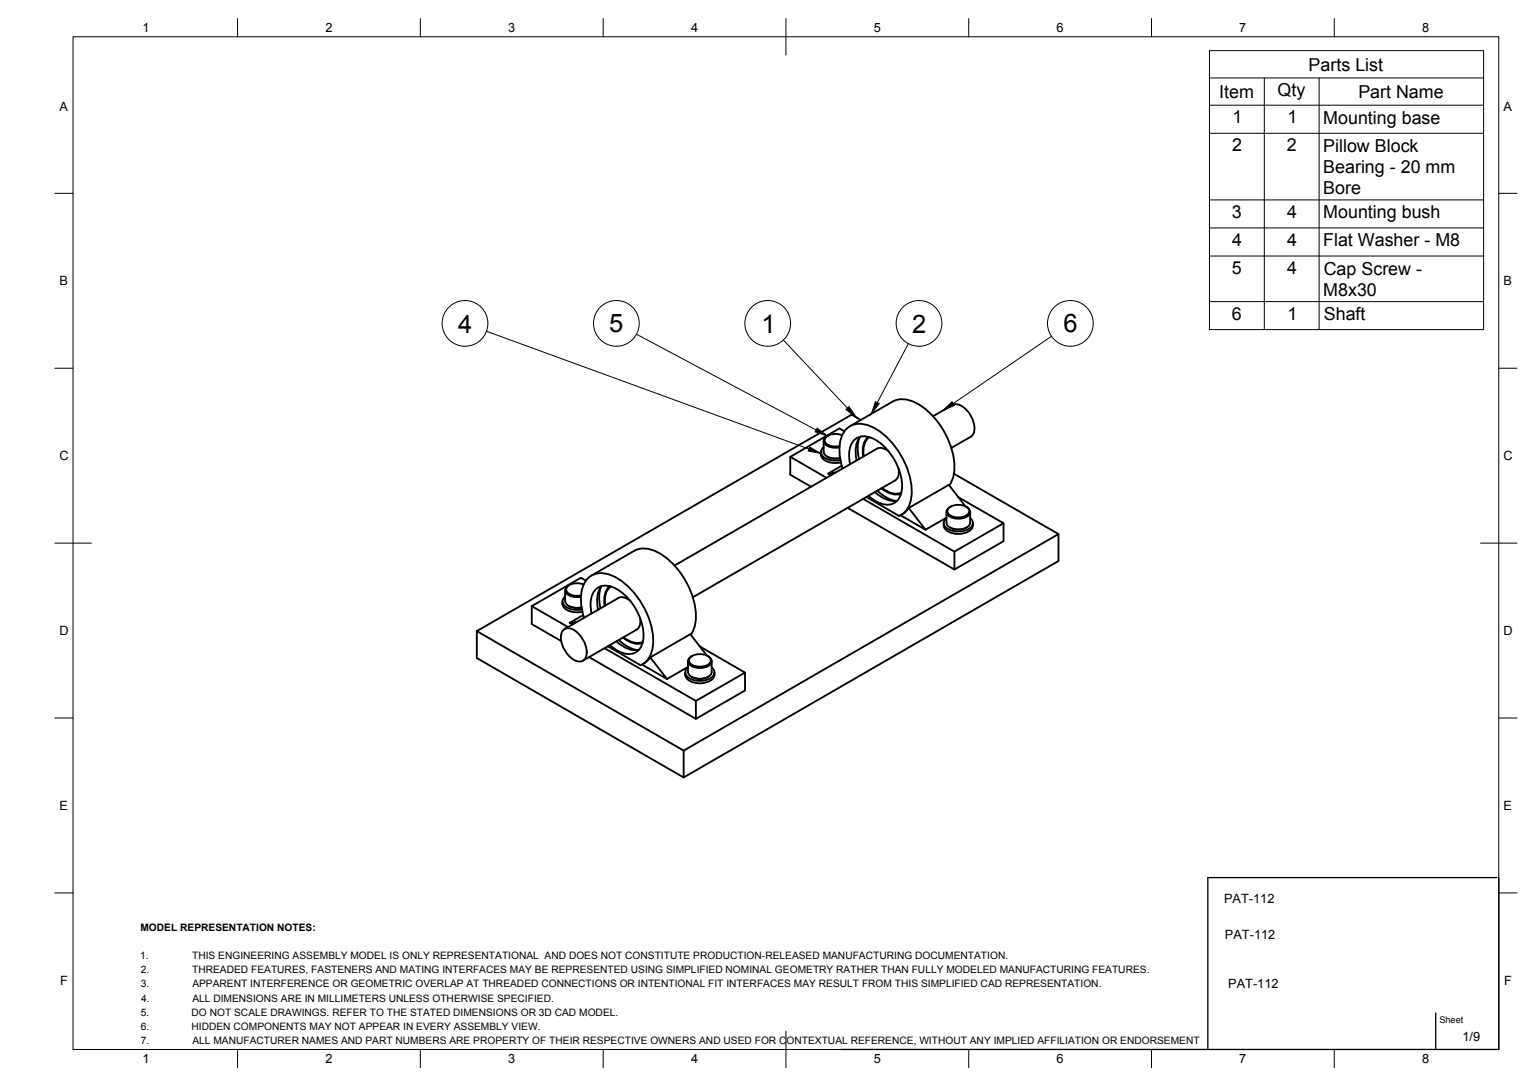
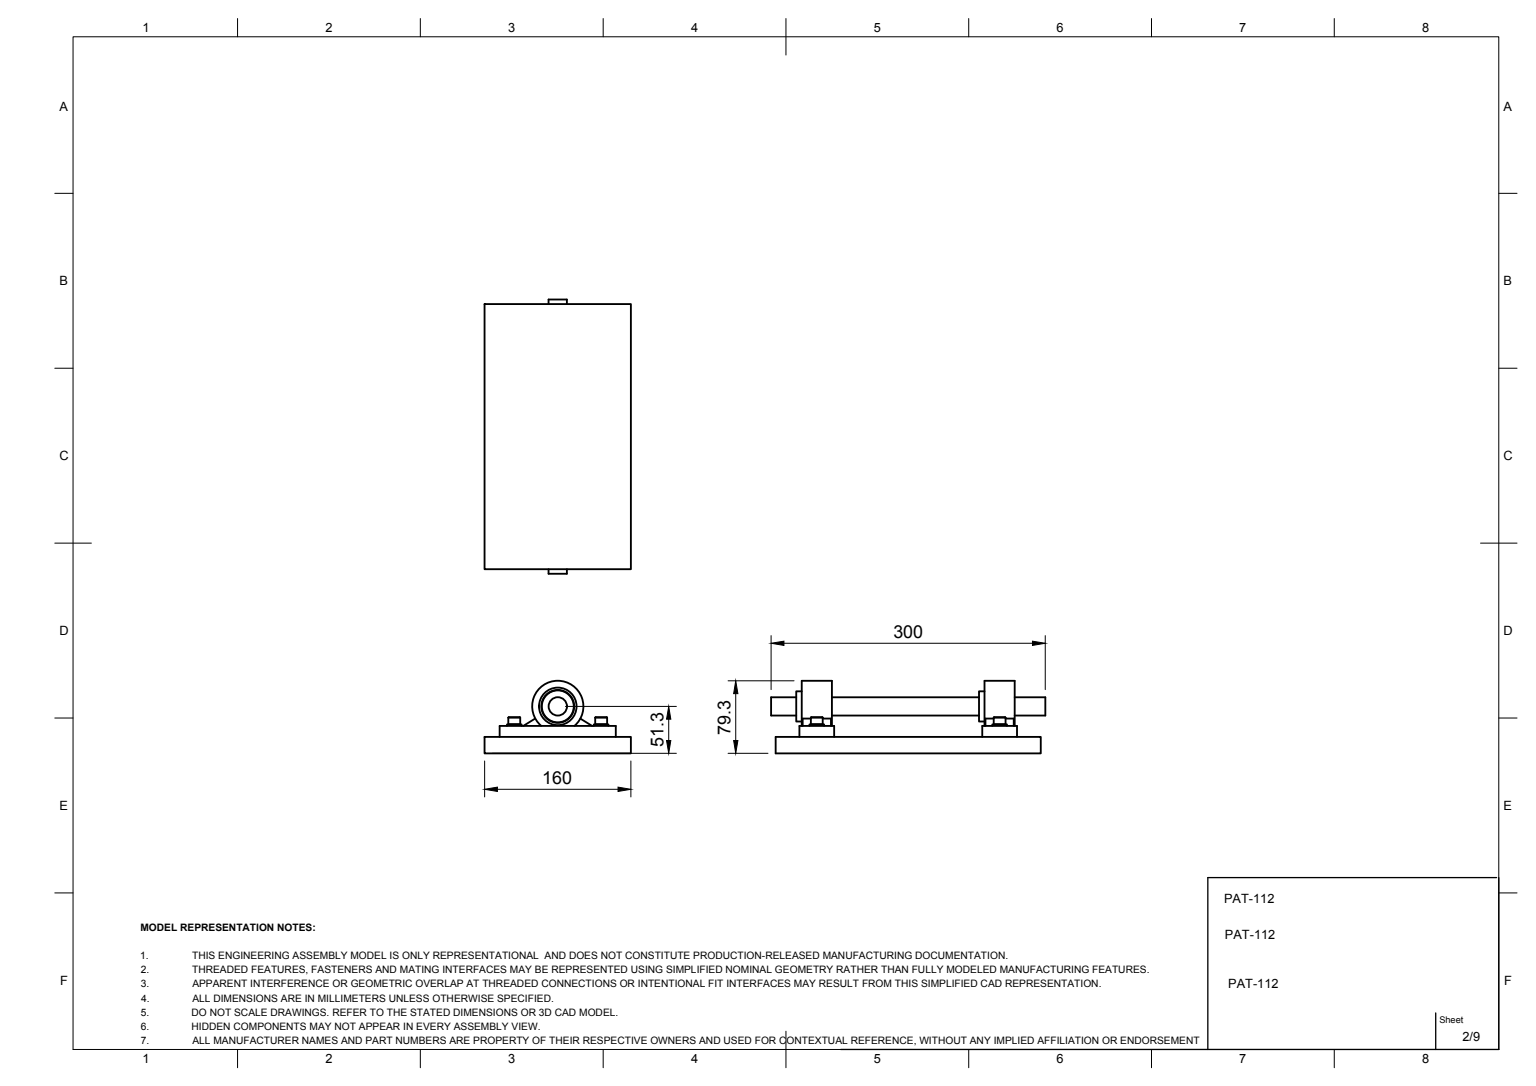
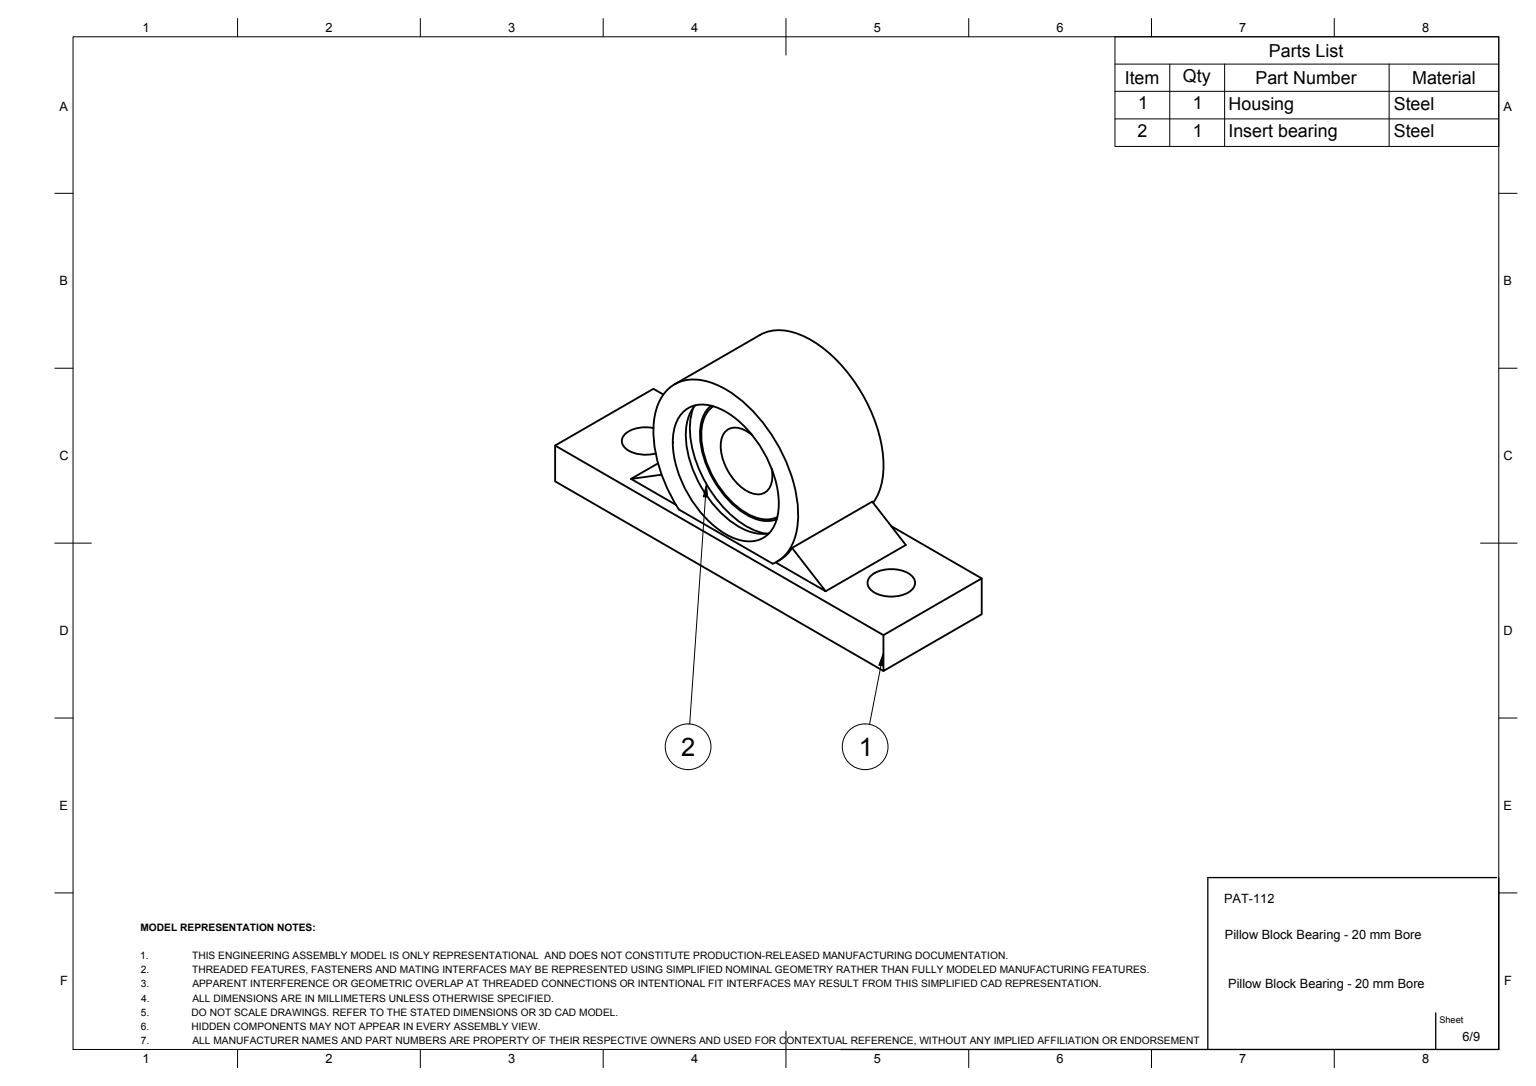
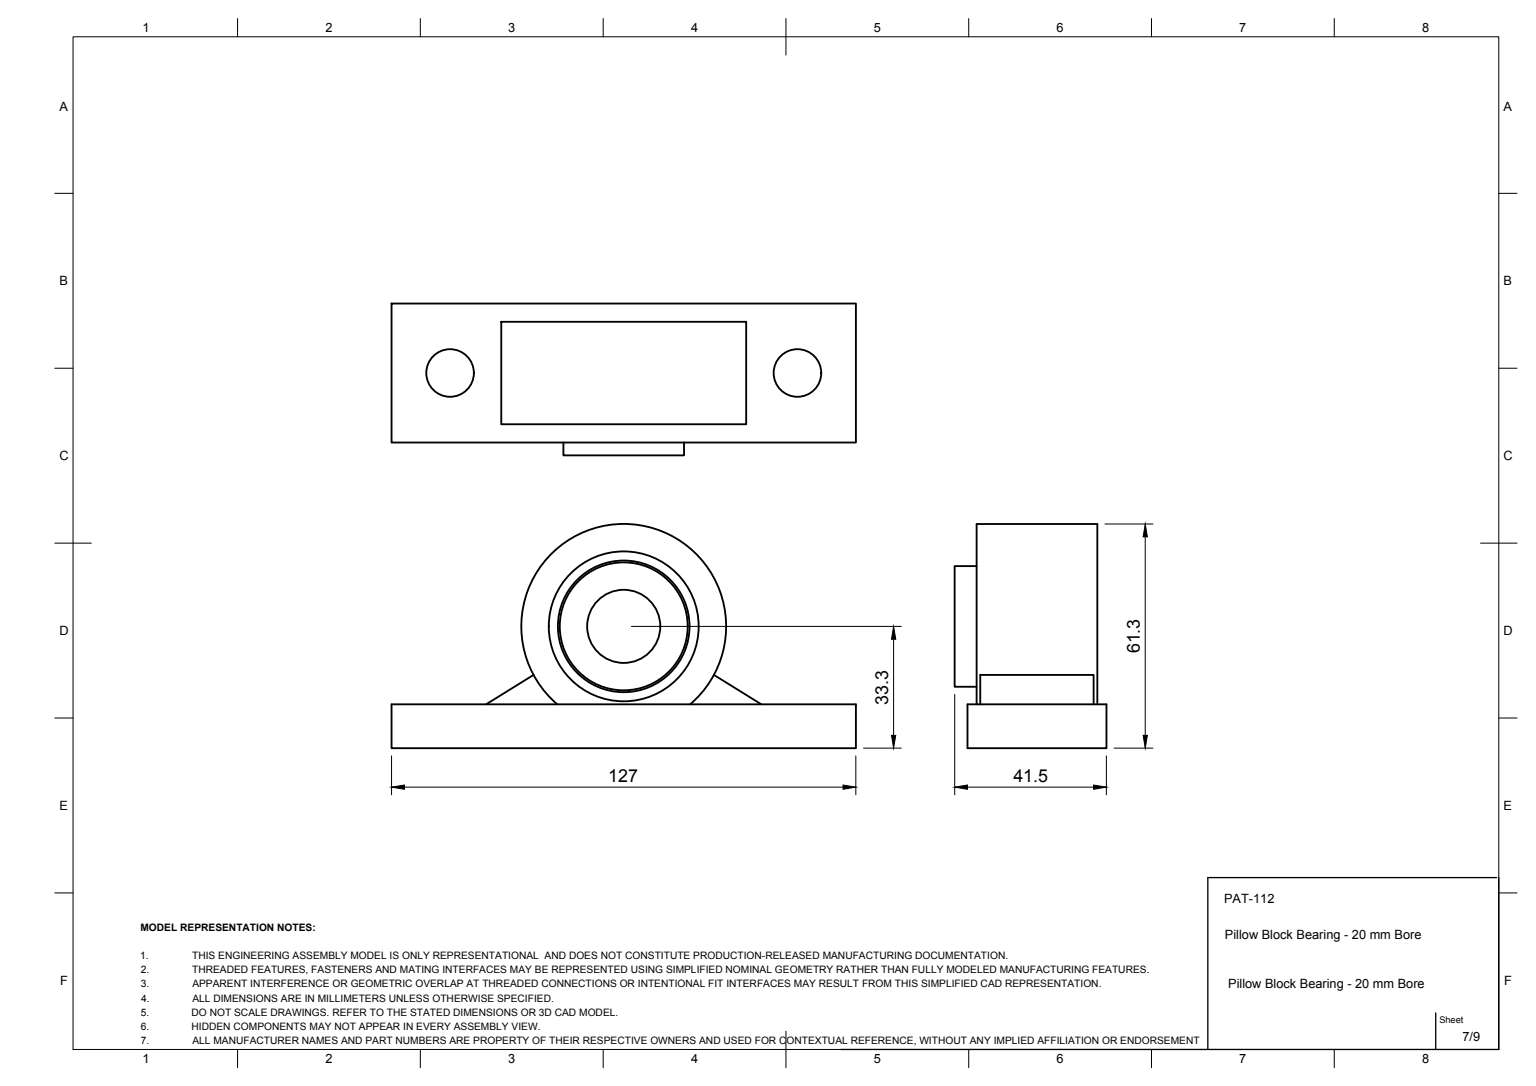
ISO-10303-21;
HEADER;
/* Generated by software containing ST-Developer
 * from STEP Tools, Inc. (www.steptools.com) 
 */

FILE_DESCRIPTION(
/* description */ ('PAT-112'),
/* implementation_level */ '2;1');

FILE_NAME(
/* name */ 'PAT-112.step',
/* time_stamp */ '2026-11-15T15:25:42-08:00',
/* author */ (''),
/* organization */ (''),
/* preprocessor_version */ 'ST-DEVELOPER v20.2',
/* originating_system */ 'Autodesk Translation Framework v15.17.0.0',
/* authorisation */ '');

FILE_SCHEMA (('AUTOMOTIVE_DESIGN { 1 0 10303 214 3 1 1 }'));
ENDSEC;

DATA;
#10=MECHANICAL_DESIGN_GEOMETRIC_PRESENTATION_REPRESENTATION('',(#105,#106,
#107,#108,#109,#110,#111,#112),#2277);
#11=CONICAL_SURFACE('',#1463,0.625,0.785398163397448);
#12=CONICAL_SURFACE('',#1467,0.635,0.785398163397449);
#13=CONICAL_SURFACE('',#1471,0.41,0.463647609000806);
#14=CONICAL_SURFACE('',#1475,0.36,0.785398163397448);
#15=ORIENTED_CLOSED_SHELL('',*,#1263,.F.);
#16=BREP_WITH_VOIDS('Body1',#1264,(#15));
#17=ITEM_DEFINED_TRANSFORMATION($,$,#1369,#1432);
#18=ITEM_DEFINED_TRANSFORMATION($,$,#1410,#1433);
#19=ITEM_DEFINED_TRANSFORMATION($,$,#1345,#1484);
#20=ITEM_DEFINED_TRANSFORMATION($,$,#1368,#1485);
#21=ITEM_DEFINED_TRANSFORMATION($,$,#1434,#1486);
#22=ITEM_DEFINED_TRANSFORMATION($,$,#1443,#1487);
#23=ITEM_DEFINED_TRANSFORMATION($,$,#1452,#1488);
#24=ITEM_DEFINED_TRANSFORMATION($,$,#1434,#1489);
#25=ITEM_DEFINED_TRANSFORMATION($,$,#1443,#1490);
#26=ITEM_DEFINED_TRANSFORMATION($,$,#1452,#1491);
#27=ITEM_DEFINED_TRANSFORMATION($,$,#1368,#1492);
#28=ITEM_DEFINED_TRANSFORMATION($,$,#1434,#1493);
#29=ITEM_DEFINED_TRANSFORMATION($,$,#1443,#1494);
#30=ITEM_DEFINED_TRANSFORMATION($,$,#1452,#1495);
#31=ITEM_DEFINED_TRANSFORMATION($,$,#1434,#1496);
#32=ITEM_DEFINED_TRANSFORMATION($,$,#1443,#1497);
#33=ITEM_DEFINED_TRANSFORMATION($,$,#1452,#1498);
#34=ITEM_DEFINED_TRANSFORMATION($,$,#1478,#1499);
#35=(
REPRESENTATION_RELATIONSHIP($,$,#2321,#2320)
REPRESENTATION_RELATIONSHIP_WITH_TRANSFORMATION(#17)
SHAPE_REPRESENTATION_RELATIONSHIP()
);
#36=(
REPRESENTATION_RELATIONSHIP($,$,#2322,#2320)
REPRESENTATION_RELATIONSHIP_WITH_TRANSFORMATION(#18)
SHAPE_REPRESENTATION_RELATIONSHIP()
);
#37=(
REPRESENTATION_RELATIONSHIP($,$,#2319,#2318)
REPRESENTATION_RELATIONSHIP_WITH_TRANSFORMATION(#19)
SHAPE_REPRESENTATION_RELATIONSHIP()
);
#38=(
REPRESENTATION_RELATIONSHIP($,$,#2320,#2318)
REPRESENTATION_RELATIONSHIP_WITH_TRANSFORMATION(#20)
SHAPE_REPRESENTATION_RELATIONSHIP()
);
#39=(
REPRESENTATION_RELATIONSHIP($,$,#2323,#2318)
REPRESENTATION_RELATIONSHIP_WITH_TRANSFORMATION(#21)
SHAPE_REPRESENTATION_RELATIONSHIP()
);
#40=(
REPRESENTATION_RELATIONSHIP($,$,#2324,#2318)
REPRESENTATION_RELATIONSHIP_WITH_TRANSFORMATION(#22)
SHAPE_REPRESENTATION_RELATIONSHIP()
);
#41=(
REPRESENTATION_RELATIONSHIP($,$,#2325,#2318)
REPRESENTATION_RELATIONSHIP_WITH_TRANSFORMATION(#23)
SHAPE_REPRESENTATION_RELATIONSHIP()
);
#42=(
REPRESENTATION_RELATIONSHIP($,$,#2323,#2318)
REPRESENTATION_RELATIONSHIP_WITH_TRANSFORMATION(#24)
SHAPE_REPRESENTATION_RELATIONSHIP()
);
#43=(
REPRESENTATION_RELATIONSHIP($,$,#2324,#2318)
REPRESENTATION_RELATIONSHIP_WITH_TRANSFORMATION(#25)
SHAPE_REPRESENTATION_RELATIONSHIP()
);
#44=(
REPRESENTATION_RELATIONSHIP($,$,#2325,#2318)
REPRESENTATION_RELATIONSHIP_WITH_TRANSFORMATION(#26)
SHAPE_REPRESENTATION_RELATIONSHIP()
);
#45=(
REPRESENTATION_RELATIONSHIP($,$,#2320,#2318)
REPRESENTATION_RELATIONSHIP_WITH_TRANSFORMATION(#27)
SHAPE_REPRESENTATION_RELATIONSHIP()
);
#46=(
REPRESENTATION_RELATIONSHIP($,$,#2323,#2318)
REPRESENTATION_RELATIONSHIP_WITH_TRANSFORMATION(#28)
SHAPE_REPRESENTATION_RELATIONSHIP()
);
#47=(
REPRESENTATION_RELATIONSHIP($,$,#2324,#2318)
REPRESENTATION_RELATIONSHIP_WITH_TRANSFORMATION(#29)
SHAPE_REPRESENTATION_RELATIONSHIP()
);
#48=(
REPRESENTATION_RELATIONSHIP($,$,#2325,#2318)
REPRESENTATION_RELATIONSHIP_WITH_TRANSFORMATION(#30)
SHAPE_REPRESENTATION_RELATIONSHIP()
);
#49=(
REPRESENTATION_RELATIONSHIP($,$,#2323,#2318)
REPRESENTATION_RELATIONSHIP_WITH_TRANSFORMATION(#31)
SHAPE_REPRESENTATION_RELATIONSHIP()
);
#50=(
REPRESENTATION_RELATIONSHIP($,$,#2324,#2318)
REPRESENTATION_RELATIONSHIP_WITH_TRANSFORMATION(#32)
SHAPE_REPRESENTATION_RELATIONSHIP()
);
#51=(
REPRESENTATION_RELATIONSHIP($,$,#2325,#2318)
REPRESENTATION_RELATIONSHIP_WITH_TRANSFORMATION(#33)
SHAPE_REPRESENTATION_RELATIONSHIP()
);
#52=(
REPRESENTATION_RELATIONSHIP($,$,#2326,#2318)
REPRESENTATION_RELATIONSHIP_WITH_TRANSFORMATION(#34)
SHAPE_REPRESENTATION_RELATIONSHIP()
);
#53=CONTEXT_DEPENDENT_SHAPE_REPRESENTATION(#35,#2296);
#54=CONTEXT_DEPENDENT_SHAPE_REPRESENTATION(#36,#2297);
#55=CONTEXT_DEPENDENT_SHAPE_REPRESENTATION(#37,#2302);
#56=CONTEXT_DEPENDENT_SHAPE_REPRESENTATION(#38,#2303);
#57=CONTEXT_DEPENDENT_SHAPE_REPRESENTATION(#39,#2304);
#58=CONTEXT_DEPENDENT_SHAPE_REPRESENTATION(#40,#2305);
#59=CONTEXT_DEPENDENT_SHAPE_REPRESENTATION(#41,#2306);
#60=CONTEXT_DEPENDENT_SHAPE_REPRESENTATION(#42,#2307);
#61=CONTEXT_DEPENDENT_SHAPE_REPRESENTATION(#43,#2308);
#62=CONTEXT_DEPENDENT_SHAPE_REPRESENTATION(#44,#2309);
#63=CONTEXT_DEPENDENT_SHAPE_REPRESENTATION(#45,#2310);
#64=CONTEXT_DEPENDENT_SHAPE_REPRESENTATION(#46,#2311);
#65=CONTEXT_DEPENDENT_SHAPE_REPRESENTATION(#47,#2312);
#66=CONTEXT_DEPENDENT_SHAPE_REPRESENTATION(#48,#2313);
#67=CONTEXT_DEPENDENT_SHAPE_REPRESENTATION(#49,#2314);
#68=CONTEXT_DEPENDENT_SHAPE_REPRESENTATION(#50,#2315);
#69=CONTEXT_DEPENDENT_SHAPE_REPRESENTATION(#51,#2316);
#70=CONTEXT_DEPENDENT_SHAPE_REPRESENTATION(#52,#2317);
#71=NEXT_ASSEMBLY_USAGE_OCCURRENCE('Housing:1','Housing:1','Housing:1',
#2330,#2331,'Housing:1');
#72=NEXT_ASSEMBLY_USAGE_OCCURRENCE('Insert bearing:1',
'Insert bearing:1','Insert bearing:1',#2330,#2332,'Insert bearing:1');
#73=NEXT_ASSEMBLY_USAGE_OCCURRENCE('Mounting base:1','Mounting base:1',
'Mounting base:1',#2328,#2329,'Mounting base:1');
#74=NEXT_ASSEMBLY_USAGE_OCCURRENCE(
'Pillow Block Bearing - 20 mm Bore:1',
'Pillow Block Bearing - 20 mm Bore:1',
'Pillow Block Bearing - 20 mm Bore:1',#2328,#2330,
'Pillow Block Bearing - 20 mm Bore:1');
#75=NEXT_ASSEMBLY_USAGE_OCCURRENCE('Mounting bush:1','Mounting bush:1',
'Mounting bush:1',#2328,#2333,'Mounting bush:1');
#76=NEXT_ASSEMBLY_USAGE_OCCURRENCE('Flat Washer - M8:1',
'Flat Washer - M8:1','Flat Washer - M8:1',#2328,#2334,
'Flat Washer - M8:1');
#77=NEXT_ASSEMBLY_USAGE_OCCURRENCE('Cap Screw - M8x30:1',
'Cap Screw - M8x30:1','Cap Screw - M8x30:1',#2328,#2335,
'Cap Screw - M8x30:1');
#78=NEXT_ASSEMBLY_USAGE_OCCURRENCE('Mounting bush:2','Mounting bush:2',
'Mounting bush:2',#2328,#2333,'Mounting bush:2');
#79=NEXT_ASSEMBLY_USAGE_OCCURRENCE('Flat Washer - M8:2',
'Flat Washer - M8:2','Flat Washer - M8:2',#2328,#2334,
'Flat Washer - M8:2');
#80=NEXT_ASSEMBLY_USAGE_OCCURRENCE('Cap Screw - M8x30:2',
'Cap Screw - M8x30:2','Cap Screw - M8x30:2',#2328,#2335,
'Cap Screw - M8x30:2');
#81=NEXT_ASSEMBLY_USAGE_OCCURRENCE(
'Pillow Block Bearing - 20 mm Bore:2',
'Pillow Block Bearing - 20 mm Bore:2',
'Pillow Block Bearing - 20 mm Bore:2',#2328,#2330,
'Pillow Block Bearing - 20 mm Bore:2');
#82=NEXT_ASSEMBLY_USAGE_OCCURRENCE('Mounting bush:3','Mounting bush:3',
'Mounting bush:3',#2328,#2333,'Mounting bush:3');
#83=NEXT_ASSEMBLY_USAGE_OCCURRENCE('Flat Washer - M8:3',
'Flat Washer - M8:3','Flat Washer - M8:3',#2328,#2334,
'Flat Washer - M8:3');
#84=NEXT_ASSEMBLY_USAGE_OCCURRENCE('Cap Screw - M8x30:3',
'Cap Screw - M8x30:3','Cap Screw - M8x30:3',#2328,#2335,
'Cap Screw - M8x30:3');
#85=NEXT_ASSEMBLY_USAGE_OCCURRENCE('Mounting bush:4','Mounting bush:4',
'Mounting bush:4',#2328,#2333,'Mounting bush:4');
#86=NEXT_ASSEMBLY_USAGE_OCCURRENCE('Flat Washer - M8:4',
'Flat Washer - M8:4','Flat Washer - M8:4',#2328,#2334,
'Flat Washer - M8:4');
#87=NEXT_ASSEMBLY_USAGE_OCCURRENCE('Cap Screw - M8x30:4',
'Cap Screw - M8x30:4','Cap Screw - M8x30:4',#2328,#2335,
'Cap Screw - M8x30:4');
#88=NEXT_ASSEMBLY_USAGE_OCCURRENCE('Shaft:1','Shaft:1','Shaft:1',#2328,
#2336,'Shaft:1');
#89=SPHERICAL_SURFACE('',#1376,2.35);
#90=SPHERICAL_SURFACE('',#1416,2.35);
#91=SHAPE_REPRESENTATION_RELATIONSHIP('SRR','None',#2319,#98);
#92=SHAPE_REPRESENTATION_RELATIONSHIP('SRR','None',#2321,#99);
#93=SHAPE_REPRESENTATION_RELATIONSHIP('SRR','None',#2322,#100);
#94=SHAPE_REPRESENTATION_RELATIONSHIP('SRR','None',#2323,#101);
#95=SHAPE_REPRESENTATION_RELATIONSHIP('SRR','None',#2324,#102);
#96=SHAPE_REPRESENTATION_RELATIONSHIP('SRR','None',#2325,#103);
#97=SHAPE_REPRESENTATION_RELATIONSHIP('SRR','None',#2326,#104);
#98=ADVANCED_BREP_SHAPE_REPRESENTATION('',(#113),#2269);
#99=ADVANCED_BREP_SHAPE_REPRESENTATION('',(#114),#2271);
#100=ADVANCED_BREP_SHAPE_REPRESENTATION('',(#115,#116),#2272);
#101=ADVANCED_BREP_SHAPE_REPRESENTATION('',(#117),#2273);
#102=ADVANCED_BREP_SHAPE_REPRESENTATION('',(#118),#2274);
#103=ADVANCED_BREP_SHAPE_REPRESENTATION('',(#16),#2275);
#104=ADVANCED_BREP_SHAPE_REPRESENTATION('',(#119),#2276);
#105=STYLED_ITEM('',(#2368),#113);
#106=STYLED_ITEM('',(#2368),#114);
#107=STYLED_ITEM('',(#2369),#115);
#108=STYLED_ITEM('',(#2369),#116);
#109=STYLED_ITEM('',(#2370),#117);
#110=STYLED_ITEM('',(#2371),#118);
#111=STYLED_ITEM('',(#2371),#16);
#112=STYLED_ITEM('',(#2367),#119);
#113=MANIFOLD_SOLID_BREP('Body1',#1257);
#114=MANIFOLD_SOLID_BREP('Body1',#1258);
#115=MANIFOLD_SOLID_BREP('Body1',#1259);
#116=MANIFOLD_SOLID_BREP('Body2',#1260);
#117=MANIFOLD_SOLID_BREP('Body1',#1261);
#118=MANIFOLD_SOLID_BREP('Body1',#1262);
#119=MANIFOLD_SOLID_BREP('Body1',#1265);
#120=FACE_BOUND('',#287,.T.);
#121=FACE_BOUND('',#288,.T.);
#122=FACE_BOUND('',#289,.T.);
#123=FACE_BOUND('',#290,.T.);
#124=FACE_BOUND('',#295,.T.);
#125=FACE_BOUND('',#296,.T.);
#126=FACE_BOUND('',#304,.T.);
#127=FACE_BOUND('',#305,.T.);
#128=FACE_BOUND('',#306,.T.);
#129=FACE_BOUND('',#309,.T.);
#130=FACE_BOUND('',#311,.T.);
#131=FACE_BOUND('',#324,.T.);
#132=FACE_BOUND('',#325,.T.);
#133=FACE_BOUND('',#326,.T.);
#134=FACE_BOUND('',#329,.T.);
#135=FACE_BOUND('',#331,.T.);
#136=FACE_BOUND('',#332,.T.);
#137=FACE_BOUND('',#334,.T.);
#138=FACE_BOUND('',#337,.T.);
#139=FACE_BOUND('',#339,.T.);
#140=FACE_BOUND('',#342,.T.);
#141=FACE_BOUND('',#347,.T.);
#142=FACE_BOUND('',#349,.T.);
#143=FACE_BOUND('',#353,.T.);
#144=FACE_BOUND('',#355,.T.);
#145=FACE_BOUND('',#369,.T.);
#146=PLANE('',#1349);
#147=PLANE('',#1353);
#148=PLANE('',#1357);
#149=PLANE('',#1361);
#150=PLANE('',#1362);
#151=PLANE('',#1363);
#152=PLANE('',#1364);
#153=PLANE('',#1365);
#154=PLANE('',#1366);
#155=PLANE('',#1367);
#156=PLANE('',#1378);
#157=PLANE('',#1380);
#158=PLANE('',#1382);
#159=PLANE('',#1384);
#160=PLANE('',#1385);
#161=PLANE('',#1387);
#162=PLANE('',#1388);
#163=PLANE('',#1394);
#164=PLANE('',#1395);
#165=PLANE('',#1396);
#166=PLANE('',#1397);
#167=PLANE('',#1398);
#168=PLANE('',#1399);
#169=PLANE('',#1400);
#170=PLANE('',#1405);
#171=PLANE('',#1406);
#172=PLANE('',#1407);
#173=PLANE('',#1408);
#174=PLANE('',#1409);
#175=PLANE('',#1414);
#176=PLANE('',#1419);
#177=PLANE('',#1423);
#178=PLANE('',#1425);
#179=PLANE('',#1429);
#180=PLANE('',#1441);
#181=PLANE('',#1442);
#182=PLANE('',#1450);
#183=PLANE('',#1451);
#184=PLANE('',#1453);
#185=PLANE('',#1454);
#186=PLANE('',#1455);
#187=PLANE('',#1456);
#188=PLANE('',#1457);
#189=PLANE('',#1458);
#190=PLANE('',#1459);
#191=PLANE('',#1460);
#192=PLANE('',#1461);
#193=PLANE('',#1469);
#194=PLANE('',#1477);
#195=PLANE('',#1479);
#196=PLANE('',#1483);
#197=FACE_OUTER_BOUND('',#274,.T.);
#198=FACE_OUTER_BOUND('',#275,.T.);
#199=FACE_OUTER_BOUND('',#276,.T.);
#200=FACE_OUTER_BOUND('',#277,.T.);
#201=FACE_OUTER_BOUND('',#278,.T.);
#202=FACE_OUTER_BOUND('',#279,.T.);
#203=FACE_OUTER_BOUND('',#280,.T.);
#204=FACE_OUTER_BOUND('',#281,.T.);
#205=FACE_OUTER_BOUND('',#282,.T.);
#206=FACE_OUTER_BOUND('',#283,.T.);
#207=FACE_OUTER_BOUND('',#284,.T.);
#208=FACE_OUTER_BOUND('',#285,.T.);
#209=FACE_OUTER_BOUND('',#286,.T.);
#210=FACE_OUTER_BOUND('',#291,.T.);
#211=FACE_OUTER_BOUND('',#292,.T.);
#212=FACE_OUTER_BOUND('',#293,.T.);
#213=FACE_OUTER_BOUND('',#294,.T.);
#214=FACE_OUTER_BOUND('',#297,.T.);
#215=FACE_OUTER_BOUND('',#298,.T.);
#216=FACE_OUTER_BOUND('',#299,.T.);
#217=FACE_OUTER_BOUND('',#300,.T.);
#218=FACE_OUTER_BOUND('',#301,.T.);
#219=FACE_OUTER_BOUND('',#302,.T.);
#220=FACE_OUTER_BOUND('',#303,.T.);
#221=FACE_OUTER_BOUND('',#307,.T.);
#222=FACE_OUTER_BOUND('',#308,.T.);
#223=FACE_OUTER_BOUND('',#310,.T.);
#224=FACE_OUTER_BOUND('',#312,.T.);
#225=FACE_OUTER_BOUND('',#313,.T.);
#226=FACE_OUTER_BOUND('',#314,.T.);
#227=FACE_OUTER_BOUND('',#315,.T.);
#228=FACE_OUTER_BOUND('',#316,.T.);
#229=FACE_OUTER_BOUND('',#317,.T.);
#230=FACE_OUTER_BOUND('',#318,.T.);
#231=FACE_OUTER_BOUND('',#319,.T.);
#232=FACE_OUTER_BOUND('',#320,.T.);
#233=FACE_OUTER_BOUND('',#321,.T.);
#234=FACE_OUTER_BOUND('',#322,.T.);
#235=FACE_OUTER_BOUND('',#323,.T.);
#236=FACE_OUTER_BOUND('',#327,.T.);
#237=FACE_OUTER_BOUND('',#328,.T.);
#238=FACE_OUTER_BOUND('',#330,.T.);
#239=FACE_OUTER_BOUND('',#333,.T.);
#240=FACE_OUTER_BOUND('',#335,.T.);
#241=FACE_OUTER_BOUND('',#336,.T.);
#242=FACE_OUTER_BOUND('',#338,.T.);
#243=FACE_OUTER_BOUND('',#340,.T.);
#244=FACE_OUTER_BOUND('',#341,.T.);
#245=FACE_OUTER_BOUND('',#343,.T.);
#246=FACE_OUTER_BOUND('',#344,.T.);
#247=FACE_OUTER_BOUND('',#345,.T.);
#248=FACE_OUTER_BOUND('',#346,.T.);
#249=FACE_OUTER_BOUND('',#348,.T.);
#250=FACE_OUTER_BOUND('',#350,.T.);
#251=FACE_OUTER_BOUND('',#351,.T.);
#252=FACE_OUTER_BOUND('',#352,.T.);
#253=FACE_OUTER_BOUND('',#354,.T.);
#254=FACE_OUTER_BOUND('',#356,.T.);
#255=FACE_OUTER_BOUND('',#357,.T.);
#256=FACE_OUTER_BOUND('',#358,.T.);
#257=FACE_OUTER_BOUND('',#359,.T.);
#258=FACE_OUTER_BOUND('',#360,.T.);
#259=FACE_OUTER_BOUND('',#361,.T.);
#260=FACE_OUTER_BOUND('',#362,.T.);
#261=FACE_OUTER_BOUND('',#363,.T.);
#262=FACE_OUTER_BOUND('',#364,.T.);
#263=FACE_OUTER_BOUND('',#365,.T.);
#264=FACE_OUTER_BOUND('',#366,.T.);
#265=FACE_OUTER_BOUND('',#367,.T.);
#266=FACE_OUTER_BOUND('',#368,.T.);
#267=FACE_OUTER_BOUND('',#370,.T.);
#268=FACE_OUTER_BOUND('',#371,.T.);
#269=FACE_OUTER_BOUND('',#372,.T.);
#270=FACE_OUTER_BOUND('',#373,.T.);
#271=FACE_OUTER_BOUND('',#374,.T.);
#272=FACE_OUTER_BOUND('',#375,.T.);
#273=FACE_OUTER_BOUND('',#376,.T.);
#274=EDGE_LOOP('',(#866,#867,#868,#869));
#275=EDGE_LOOP('',(#870));
#276=EDGE_LOOP('',(#871,#872,#873,#874));
#277=EDGE_LOOP('',(#875));
#278=EDGE_LOOP('',(#876,#877,#878,#879));
#279=EDGE_LOOP('',(#880));
#280=EDGE_LOOP('',(#881,#882,#883,#884));
#281=EDGE_LOOP('',(#885));
#282=EDGE_LOOP('',(#886,#887,#888,#889));
#283=EDGE_LOOP('',(#890,#891,#892,#893));
#284=EDGE_LOOP('',(#894,#895,#896,#897));
#285=EDGE_LOOP('',(#898,#899,#900,#901));
#286=EDGE_LOOP('',(#902,#903,#904,#905));
#287=EDGE_LOOP('',(#906));
#288=EDGE_LOOP('',(#907));
#289=EDGE_LOOP('',(#908));
#290=EDGE_LOOP('',(#909));
#291=EDGE_LOOP('',(#910,#911,#912,#913));
#292=EDGE_LOOP('',(#914,#915,#916,#917));
#293=EDGE_LOOP('',(#918,#919,#920,#921));
#294=EDGE_LOOP('',(#922,#923));
#295=EDGE_LOOP('',(#924));
#296=EDGE_LOOP('',(#925));
#297=EDGE_LOOP('',(#926,#927,#928));
#298=EDGE_LOOP('',(#929,#930,#931));
#299=EDGE_LOOP('',(#932,#933,#934));
#300=EDGE_LOOP('',(#935,#936,#937,#938));
#301=EDGE_LOOP('',(#939,#940,#941));
#302=EDGE_LOOP('',(#942,#943,#944,#945));
#303=EDGE_LOOP('',(#946,#947,#948,#949));
#304=EDGE_LOOP('',(#950));
#305=EDGE_LOOP('',(#951));
#306=EDGE_LOOP('',(#952,#953,#954,#955,#956,#957,#958,#959,#960,#961,#962,
#963));
#307=EDGE_LOOP('',(#964,#965,#966,#967,#968,#969,#970,#971,#972,#973,#974,
#975));
#308=EDGE_LOOP('',(#976,#977));
#309=EDGE_LOOP('',(#978));
#310=EDGE_LOOP('',(#979,#980));
#311=EDGE_LOOP('',(#981));
#312=EDGE_LOOP('',(#982,#983,#984,#985));
#313=EDGE_LOOP('',(#986,#987,#988,#989));
#314=EDGE_LOOP('',(#990,#991,#992,#993));
#315=EDGE_LOOP('',(#994,#995,#996,#997));
#316=EDGE_LOOP('',(#998,#999,#1000,#1001));
#317=EDGE_LOOP('',(#1002,#1003,#1004,#1005));
#318=EDGE_LOOP('',(#1006,#1007,#1008,#1009));
#319=EDGE_LOOP('',(#1010,#1011,#1012,#1013));
#320=EDGE_LOOP('',(#1014,#1015,#1016,#1017));
#321=EDGE_LOOP('',(#1018,#1019,#1020,#1021));
#322=EDGE_LOOP('',(#1022,#1023,#1024,#1025));
#323=EDGE_LOOP('',(#1026,#1027,#1028,#1029));
#324=EDGE_LOOP('',(#1030,#1031,#1032,#1033));
#325=EDGE_LOOP('',(#1034));
#326=EDGE_LOOP('',(#1035));
#327=EDGE_LOOP('',(#1036,#1037,#1038,#1039));
#328=EDGE_LOOP('',(#1040));
#329=EDGE_LOOP('',(#1041));
#330=EDGE_LOOP('',(#1042,#1043));
#331=EDGE_LOOP('',(#1044));
#332=EDGE_LOOP('',(#1045));
#333=EDGE_LOOP('',(#1046));
#334=EDGE_LOOP('',(#1047));
#335=EDGE_LOOP('',(#1048,#1049,#1050,#1051));
#336=EDGE_LOOP('',(#1052));
#337=EDGE_LOOP('',(#1053));
#338=EDGE_LOOP('',(#1054));
#339=EDGE_LOOP('',(#1055));
#340=EDGE_LOOP('',(#1056,#1057,#1058,#1059));
#341=EDGE_LOOP('',(#1060));
#342=EDGE_LOOP('',(#1061));
#343=EDGE_LOOP('',(#1062,#1063,#1064,#1065));
#344=EDGE_LOOP('',(#1066,#1067,#1068,#1069));
#345=EDGE_LOOP('',(#1070,#1071,#1072,#1073));
#346=EDGE_LOOP('',(#1074));
#347=EDGE_LOOP('',(#1075));
#348=EDGE_LOOP('',(#1076));
#349=EDGE_LOOP('',(#1077));
#350=EDGE_LOOP('',(#1078,#1079,#1080,#1081));
#351=EDGE_LOOP('',(#1082,#1083,#1084,#1085));
#352=EDGE_LOOP('',(#1086));
#353=EDGE_LOOP('',(#1087));
#354=EDGE_LOOP('',(#1088));
#355=EDGE_LOOP('',(#1089));
#356=EDGE_LOOP('',(#1090,#1091,#1092,#1093));
#357=EDGE_LOOP('',(#1094,#1095,#1096,#1097));
#358=EDGE_LOOP('',(#1098,#1099,#1100,#1101));
#359=EDGE_LOOP('',(#1102,#1103,#1104,#1105));
#360=EDGE_LOOP('',(#1106,#1107,#1108,#1109));
#361=EDGE_LOOP('',(#1110,#1111,#1112,#1113));
#362=EDGE_LOOP('',(#1114,#1115,#1116,#1117,#1118,#1119));
#363=EDGE_LOOP('',(#1120,#1121,#1122,#1123,#1124,#1125));
#364=EDGE_LOOP('',(#1126));
#365=EDGE_LOOP('',(#1127,#1128,#1129,#1130));
#366=EDGE_LOOP('',(#1131,#1132,#1133,#1134));
#367=EDGE_LOOP('',(#1135,#1136,#1137,#1138));
#368=EDGE_LOOP('',(#1139));
#369=EDGE_LOOP('',(#1140));
#370=EDGE_LOOP('',(#1141,#1142,#1143,#1144));
#371=EDGE_LOOP('',(#1145,#1146,#1147,#1148));
#372=EDGE_LOOP('',(#1149,#1150,#1151,#1152));
#373=EDGE_LOOP('',(#1153));
#374=EDGE_LOOP('',(#1154));
#375=EDGE_LOOP('',(#1155,#1156,#1157,#1158));
#376=EDGE_LOOP('',(#1159));
#377=LINE('',#1913,#472);
#378=LINE('',#1920,#473);
#379=LINE('',#1927,#474);
#380=LINE('',#1934,#475);
#381=LINE('',#1940,#476);
#382=LINE('',#1942,#477);
#383=LINE('',#1944,#478);
#384=LINE('',#1945,#479);
#385=LINE('',#1948,#480);
#386=LINE('',#1950,#481);
#387=LINE('',#1951,#482);
#388=LINE('',#1954,#483);
#389=LINE('',#1956,#484);
#390=LINE('',#1957,#485);
#391=LINE('',#1959,#486);
#392=LINE('',#1960,#487);
#393=LINE('',#1969,#488);
#394=LINE('',#1975,#489);
#395=LINE('',#1984,#490);
#396=LINE('',#1986,#491);
#397=LINE('',#1991,#492);
#398=LINE('',#1994,#493);
#399=LINE('',#1998,#494);
#400=LINE('',#2001,#495);
#401=LINE('',#2003,#496);
#402=LINE('',#2004,#497);
#403=LINE('',#2008,#498);
#404=LINE('',#2010,#499);
#405=LINE('',#2013,#500);
#406=LINE('',#2014,#501);
#407=LINE('',#2018,#502);
#408=LINE('',#2020,#503);
#409=LINE('',#2022,#504);
#410=LINE('',#2023,#505);
#411=LINE('',#2029,#506);
#412=LINE('',#2031,#507);
#413=LINE('',#2032,#508);
#414=LINE('',#2034,#509);
#415=LINE('',#2036,#510);
#416=LINE('',#2037,#511);
#417=LINE('',#2046,#512);
#418=LINE('',#2048,#513);
#419=LINE('',#2050,#514);
#420=LINE('',#2051,#515);
#421=LINE('',#2054,#516);
#422=LINE('',#2056,#517);
#423=LINE('',#2057,#518);
#424=LINE('',#2060,#519);
#425=LINE('',#2062,#520);
#426=LINE('',#2063,#521);
#427=LINE('',#2065,#522);
#428=LINE('',#2066,#523);
#429=LINE('',#2071,#524);
#430=LINE('',#2075,#525);
#431=LINE('',#2079,#526);
#432=LINE('',#2080,#527);
#433=LINE('',#2081,#528);
#434=LINE('',#2084,#529);
#435=LINE('',#2085,#530);
#436=LINE('',#2088,#531);
#437=LINE('',#2089,#532);
#438=LINE('',#2091,#533);
#439=LINE('',#2098,#534);
#440=LINE('',#2114,#535);
#441=LINE('',#2125,#536);
#442=LINE('',#2130,#537);
#443=LINE('',#2138,#538);
#444=LINE('',#2144,#539);
#445=LINE('',#2153,#540);
#446=LINE('',#2159,#541);
#447=LINE('',#2167,#542);
#448=LINE('',#2169,#543);
#449=LINE('',#2171,#544);
#450=LINE('',#2172,#545);
#451=LINE('',#2175,#546);
#452=LINE('',#2177,#547);
#453=LINE('',#2178,#548);
#454=LINE('',#2181,#549);
#455=LINE('',#2183,#550);
#456=LINE('',#2184,#551);
#457=LINE('',#2187,#552);
#458=LINE('',#2189,#553);
#459=LINE('',#2190,#554);
#460=LINE('',#2193,#555);
#461=LINE('',#2195,#556);
#462=LINE('',#2196,#557);
#463=LINE('',#2198,#558);
#464=LINE('',#2199,#559);
#465=LINE('',#2208,#560);
#466=LINE('',#2212,#561);
#467=LINE('',#2215,#562);
#468=LINE('',#2222,#563);
#469=LINE('',#2227,#564);
#470=LINE('',#2230,#565);
#471=LINE('',#2240,#566);
#472=VECTOR('',#1508,0.34);
#473=VECTOR('',#1517,0.34);
#474=VECTOR('',#1526,0.34);
#475=VECTOR('',#1535,0.34);
#476=VECTOR('',#1542,1.);
#477=VECTOR('',#1543,1.);
#478=VECTOR('',#1544,1.);
#479=VECTOR('',#1545,1.);
#480=VECTOR('',#1548,1.);
#481=VECTOR('',#1549,1.);
#482=VECTOR('',#1550,1.);
#483=VECTOR('',#1553,1.);
#484=VECTOR('',#1554,1.);
#485=VECTOR('',#1555,1.);
#486=VECTOR('',#1558,1.);
#487=VECTOR('',#1559,1.);
#488=VECTOR('',#1572,2.05);
#489=VECTOR('',#1579,2.05);
#490=VECTOR('',#1588,1.);
#491=VECTOR('',#1589,1.);
#492=VECTOR('',#1594,1.);
#493=VECTOR('',#1597,1.);
#494=VECTOR('',#1600,1.);
#495=VECTOR('',#1603,1.);
#496=VECTOR('',#1606,1.);
#497=VECTOR('',#1607,1.);
#498=VECTOR('',#1610,1.);
#499=VECTOR('',#1611,1.);
#500=VECTOR('',#1616,1.);
#501=VECTOR('',#1617,1.);
#502=VECTOR('',#1620,1.);
#503=VECTOR('',#1621,1.);
#504=VECTOR('',#1622,1.);
#505=VECTOR('',#1623,1.);
#506=VECTOR('',#1628,1.);
#507=VECTOR('',#1629,1.);
#508=VECTOR('',#1630,1.);
#509=VECTOR('',#1631,1.);
#510=VECTOR('',#1632,1.);
#511=VECTOR('',#1633,1.);
#512=VECTOR('',#1646,1.);
#513=VECTOR('',#1647,1.);
#514=VECTOR('',#1648,1.);
#515=VECTOR('',#1649,1.);
#516=VECTOR('',#1652,1.);
#517=VECTOR('',#1653,1.);
#518=VECTOR('',#1654,1.);
#519=VECTOR('',#1657,1.);
#520=VECTOR('',#1658,1.);
#521=VECTOR('',#1659,1.);
#522=VECTOR('',#1662,1.);
#523=VECTOR('',#1663,1.);
#524=VECTOR('',#1670,0.65);
#525=VECTOR('',#1675,0.65);
#526=VECTOR('',#1678,1.);
#527=VECTOR('',#1679,1.);
#528=VECTOR('',#1680,1.);
#529=VECTOR('',#1683,1.);
#530=VECTOR('',#1684,1.);
#531=VECTOR('',#1687,1.);
#532=VECTOR('',#1688,1.);
#533=VECTOR('',#1691,1.);
#534=VECTOR('',#1700,1.8);
#535=VECTOR('',#1719,1.65);
#536=VECTOR('',#1734,1.75);
#537=VECTOR('',#1741,1.);
#538=VECTOR('',#1752,0.425);
#539=VECTOR('',#1759,0.645);
#540=VECTOR('',#1772,0.42);
#541=VECTOR('',#1779,0.8);
#542=VECTOR('',#1790,1.);
#543=VECTOR('',#1791,1.);
#544=VECTOR('',#1792,1.);
#545=VECTOR('',#1793,1.);
#546=VECTOR('',#1796,1.);
#547=VECTOR('',#1797,1.);
#548=VECTOR('',#1798,1.);
#549=VECTOR('',#1801,1.);
#550=VECTOR('',#1802,1.);
#551=VECTOR('',#1803,1.);
#552=VECTOR('',#1806,1.);
#553=VECTOR('',#1807,1.);
#554=VECTOR('',#1808,1.);
#555=VECTOR('',#1811,1.);
#556=VECTOR('',#1812,1.);
#557=VECTOR('',#1813,1.);
#558=VECTOR('',#1816,1.);
#559=VECTOR('',#1817,1.);
#560=VECTOR('',#1830,0.625);
#561=VECTOR('',#1835,0.65);
#562=VECTOR('',#1838,0.635);
#563=VECTOR('',#1847,0.41);
#564=VECTOR('',#1854,0.3933);
#565=VECTOR('',#1857,0.36);
#566=VECTOR('',#1872,1.);
#567=CIRCLE('',#1347,0.34);
#568=CIRCLE('',#1348,0.34);
#569=CIRCLE('',#1351,0.34);
#570=CIRCLE('',#1352,0.34);
#571=CIRCLE('',#1355,0.34);
#572=CIRCLE('',#1356,0.34);
#573=CIRCLE('',#1359,0.34);
#574=CIRCLE('',#1360,0.34);
#575=CIRCLE('',#1371,2.05);
#576=CIRCLE('',#1372,2.05);
#577=CIRCLE('',#1374,2.05);
#578=CIRCLE('',#1375,2.05);
#579=CIRCLE('',#1377,2.35);
#580=CIRCLE('',#1379,2.8);
#581=CIRCLE('',#1381,2.8);
#582=CIRCLE('',#1383,2.8);
#583=CIRCLE('',#1386,2.8);
#584=CIRCLE('',#1389,0.65);
#585=CIRCLE('',#1390,0.65);
#586=CIRCLE('',#1392,2.8);
#587=CIRCLE('',#1393,2.8);
#588=CIRCLE('',#1402,0.65);
#589=CIRCLE('',#1404,0.65);
#590=CIRCLE('',#1412,1.8);
#591=CIRCLE('',#1413,1.8);
#592=CIRCLE('',#1415,2.19089023002066);
#593=CIRCLE('',#1417,2.35);
#594=CIRCLE('',#1418,2.19089023002066);
#595=CIRCLE('',#1421,1.65);
#596=CIRCLE('',#1422,1.65);
#597=CIRCLE('',#1424,1.);
#598=CIRCLE('',#1426,1.75);
#599=CIRCLE('',#1428,1.75);
#600=CIRCLE('',#1430,1.);
#601=CIRCLE('',#1436,0.425);
#602=CIRCLE('',#1437,0.425);
#603=CIRCLE('',#1439,0.645);
#604=CIRCLE('',#1440,0.645);
#605=CIRCLE('',#1445,0.42);
#606=CIRCLE('',#1446,0.42);
#607=CIRCLE('',#1448,0.8);
#608=CIRCLE('',#1449,0.8);
#609=CIRCLE('',#1462,0.6);
#610=CIRCLE('',#1464,0.65);
#611=CIRCLE('',#1466,0.65);
#612=CIRCLE('',#1468,0.62);
#613=CIRCLE('',#1470,0.42);
#614=CIRCLE('',#1472,0.3933);
#615=CIRCLE('',#1474,0.3933);
#616=CIRCLE('',#1476,0.32);
#617=CIRCLE('',#1480,1.);
#618=CIRCLE('',#1482,1.);
#619=VERTEX_POINT('',#1910);
#620=VERTEX_POINT('',#1912);
#621=VERTEX_POINT('',#1917);
#622=VERTEX_POINT('',#1919);
#623=VERTEX_POINT('',#1924);
#624=VERTEX_POINT('',#1926);
#625=VERTEX_POINT('',#1931);
#626=VERTEX_POINT('',#1933);
#627=VERTEX_POINT('',#1938);
#628=VERTEX_POINT('',#1939);
#629=VERTEX_POINT('',#1941);
#630=VERTEX_POINT('',#1943);
#631=VERTEX_POINT('',#1947);
#632=VERTEX_POINT('',#1949);
#633=VERTEX_POINT('',#1953);
#634=VERTEX_POINT('',#1955);
#635=VERTEX_POINT('',#1966);
#636=VERTEX_POINT('',#1968);
#637=VERTEX_POINT('',#1972);
#638=VERTEX_POINT('',#1974);
#639=VERTEX_POINT('',#1978);
#640=VERTEX_POINT('',#1979);
#641=VERTEX_POINT('',#1982);
#642=VERTEX_POINT('',#1983);
#643=VERTEX_POINT('',#1985);
#644=VERTEX_POINT('',#1989);
#645=VERTEX_POINT('',#1990);
#646=VERTEX_POINT('',#1992);
#647=VERTEX_POINT('',#1996);
#648=VERTEX_POINT('',#1997);
#649=VERTEX_POINT('',#1999);
#650=VERTEX_POINT('',#2006);
#651=VERTEX_POINT('',#2007);
#652=VERTEX_POINT('',#2009);
#653=VERTEX_POINT('',#2016);
#654=VERTEX_POINT('',#2017);
#655=VERTEX_POINT('',#2019);
#656=VERTEX_POINT('',#2021);
#657=VERTEX_POINT('',#2024);
#658=VERTEX_POINT('',#2026);
#659=VERTEX_POINT('',#2028);
#660=VERTEX_POINT('',#2030);
#661=VERTEX_POINT('',#2033);
#662=VERTEX_POINT('',#2035);
#663=VERTEX_POINT('',#2044);
#664=VERTEX_POINT('',#2045);
#665=VERTEX_POINT('',#2047);
#666=VERTEX_POINT('',#2049);
#667=VERTEX_POINT('',#2053);
#668=VERTEX_POINT('',#2055);
#669=VERTEX_POINT('',#2059);
#670=VERTEX_POINT('',#2061);
#671=VERTEX_POINT('',#2069);
#672=VERTEX_POINT('',#2073);
#673=VERTEX_POINT('',#2077);
#674=VERTEX_POINT('',#2078);
#675=VERTEX_POINT('',#2083);
#676=VERTEX_POINT('',#2087);
#677=VERTEX_POINT('',#2095);
#678=VERTEX_POINT('',#2097);
#679=VERTEX_POINT('',#2101);
#680=VERTEX_POINT('',#2104);
#681=VERTEX_POINT('',#2105);
#682=VERTEX_POINT('',#2107);
#683=VERTEX_POINT('',#2111);
#684=VERTEX_POINT('',#2113);
#685=VERTEX_POINT('',#2117);
#686=VERTEX_POINT('',#2120);
#687=VERTEX_POINT('',#2123);
#688=VERTEX_POINT('',#2127);
#689=VERTEX_POINT('',#2135);
#690=VERTEX_POINT('',#2137);
#691=VERTEX_POINT('',#2141);
#692=VERTEX_POINT('',#2143);
#693=VERTEX_POINT('',#2150);
#694=VERTEX_POINT('',#2152);
#695=VERTEX_POINT('',#2156);
#696=VERTEX_POINT('',#2158);
#697=VERTEX_POINT('',#2165);
#698=VERTEX_POINT('',#2166);
#699=VERTEX_POINT('',#2168);
#700=VERTEX_POINT('',#2170);
#701=VERTEX_POINT('',#2174);
#702=VERTEX_POINT('',#2176);
#703=VERTEX_POINT('',#2180);
#704=VERTEX_POINT('',#2182);
#705=VERTEX_POINT('',#2186);
#706=VERTEX_POINT('',#2188);
#707=VERTEX_POINT('',#2192);
#708=VERTEX_POINT('',#2194);
#709=VERTEX_POINT('',#2203);
#710=VERTEX_POINT('',#2206);
#711=VERTEX_POINT('',#2210);
#712=VERTEX_POINT('',#2214);
#713=VERTEX_POINT('',#2218);
#714=VERTEX_POINT('',#2221);
#715=VERTEX_POINT('',#2225);
#716=VERTEX_POINT('',#2229);
#717=VERTEX_POINT('',#2235);
#718=VERTEX_POINT('',#2238);
#719=EDGE_CURVE('',#619,#619,#567,.T.);
#720=EDGE_CURVE('',#619,#620,#377,.T.);
#721=EDGE_CURVE('',#620,#620,#568,.T.);
#722=EDGE_CURVE('',#621,#621,#569,.T.);
#723=EDGE_CURVE('',#621,#622,#378,.T.);
#724=EDGE_CURVE('',#622,#622,#570,.T.);
#725=EDGE_CURVE('',#623,#623,#571,.T.);
#726=EDGE_CURVE('',#623,#624,#379,.T.);
#727=EDGE_CURVE('',#624,#624,#572,.T.);
#728=EDGE_CURVE('',#625,#625,#573,.T.);
#729=EDGE_CURVE('',#625,#626,#380,.T.);
#730=EDGE_CURVE('',#626,#626,#574,.T.);
#731=EDGE_CURVE('',#627,#628,#381,.T.);
#732=EDGE_CURVE('',#628,#629,#382,.T.);
#733=EDGE_CURVE('',#630,#629,#383,.T.);
#734=EDGE_CURVE('',#627,#630,#384,.T.);
#735=EDGE_CURVE('',#631,#627,#385,.T.);
#736=EDGE_CURVE('',#632,#630,#386,.T.);
#737=EDGE_CURVE('',#631,#632,#387,.T.);
#738=EDGE_CURVE('',#633,#631,#388,.T.);
#739=EDGE_CURVE('',#634,#632,#389,.T.);
#740=EDGE_CURVE('',#633,#634,#390,.T.);
#741=EDGE_CURVE('',#628,#633,#391,.T.);
#742=EDGE_CURVE('',#629,#634,#392,.T.);
#743=EDGE_CURVE('',#635,#635,#575,.T.);
#744=EDGE_CURVE('',#635,#636,#393,.T.);
#745=EDGE_CURVE('',#636,#636,#576,.T.);
#746=EDGE_CURVE('',#637,#637,#577,.T.);
#747=EDGE_CURVE('',#637,#638,#394,.T.);
#748=EDGE_CURVE('',#638,#638,#578,.T.);
#749=EDGE_CURVE('',#639,#640,#579,.T.);
#750=EDGE_CURVE('',#641,#642,#395,.T.);
#751=EDGE_CURVE('',#641,#643,#396,.T.);
#752=EDGE_CURVE('',#642,#643,#580,.T.);
#753=EDGE_CURVE('',#644,#645,#397,.T.);
#754=EDGE_CURVE('',#646,#644,#581,.T.);
#755=EDGE_CURVE('',#646,#645,#398,.T.);
#756=EDGE_CURVE('',#647,#648,#399,.T.);
#757=EDGE_CURVE('',#649,#647,#582,.T.);
#758=EDGE_CURVE('',#649,#648,#400,.T.);
#759=EDGE_CURVE('',#648,#641,#401,.T.);
#760=EDGE_CURVE('',#643,#649,#402,.T.);
#761=EDGE_CURVE('',#650,#651,#403,.T.);
#762=EDGE_CURVE('',#650,#652,#404,.T.);
#763=EDGE_CURVE('',#651,#652,#583,.T.);
#764=EDGE_CURVE('',#645,#650,#405,.T.);
#765=EDGE_CURVE('',#652,#646,#406,.T.);
#766=EDGE_CURVE('',#653,#654,#407,.T.);
#767=EDGE_CURVE('',#654,#655,#408,.T.);
#768=EDGE_CURVE('',#655,#656,#409,.T.);
#769=EDGE_CURVE('',#656,#653,#410,.T.);
#770=EDGE_CURVE('',#657,#657,#584,.T.);
#771=EDGE_CURVE('',#658,#658,#585,.T.);
#772=EDGE_CURVE('',#651,#659,#411,.T.);
#773=EDGE_CURVE('',#659,#660,#412,.T.);
#774=EDGE_CURVE('',#660,#647,#413,.T.);
#775=EDGE_CURVE('',#642,#661,#414,.T.);
#776=EDGE_CURVE('',#661,#662,#415,.T.);
#777=EDGE_CURVE('',#662,#644,#416,.T.);
#778=EDGE_CURVE('',#661,#662,#586,.T.);
#779=EDGE_CURVE('',#659,#660,#587,.T.);
#780=EDGE_CURVE('',#663,#664,#417,.T.);
#781=EDGE_CURVE('',#663,#665,#418,.T.);
#782=EDGE_CURVE('',#665,#666,#419,.T.);
#783=EDGE_CURVE('',#664,#666,#420,.T.);
#784=EDGE_CURVE('',#667,#663,#421,.T.);
#785=EDGE_CURVE('',#667,#668,#422,.T.);
#786=EDGE_CURVE('',#668,#665,#423,.T.);
#787=EDGE_CURVE('',#669,#667,#424,.T.);
#788=EDGE_CURVE('',#669,#670,#425,.T.);
#789=EDGE_CURVE('',#670,#668,#426,.T.);
#790=EDGE_CURVE('',#664,#669,#427,.T.);
#791=EDGE_CURVE('',#666,#670,#428,.T.);
#792=EDGE_CURVE('',#671,#671,#588,.T.);
#793=EDGE_CURVE('',#671,#658,#429,.T.);
#794=EDGE_CURVE('',#672,#672,#589,.T.);
#795=EDGE_CURVE('',#672,#657,#430,.T.);
#796=EDGE_CURVE('',#673,#674,#431,.T.);
#797=EDGE_CURVE('',#674,#653,#432,.T.);
#798=EDGE_CURVE('',#673,#656,#433,.T.);
#799=EDGE_CURVE('',#675,#673,#434,.T.);
#800=EDGE_CURVE('',#675,#655,#435,.T.);
#801=EDGE_CURVE('',#676,#675,#436,.T.);
#802=EDGE_CURVE('',#676,#654,#437,.T.);
#803=EDGE_CURVE('',#674,#676,#438,.T.);
#804=EDGE_CURVE('',#677,#677,#590,.T.);
#805=EDGE_CURVE('',#677,#678,#439,.T.);
#806=EDGE_CURVE('',#678,#678,#591,.T.);
#807=EDGE_CURVE('',#679,#679,#592,.T.);
#808=EDGE_CURVE('',#680,#681,#593,.T.);
#809=EDGE_CURVE('',#682,#682,#594,.T.);
#810=EDGE_CURVE('',#683,#683,#595,.T.);
#811=EDGE_CURVE('',#683,#684,#440,.T.);
#812=EDGE_CURVE('',#684,#684,#596,.T.);
#813=EDGE_CURVE('',#685,#685,#597,.T.);
#814=EDGE_CURVE('',#686,#686,#598,.T.);
#815=EDGE_CURVE('',#687,#687,#599,.T.);
#816=EDGE_CURVE('',#687,#686,#441,.T.);
#817=EDGE_CURVE('',#688,#688,#600,.T.);
#818=EDGE_CURVE('',#685,#688,#442,.T.);
#819=EDGE_CURVE('',#689,#689,#601,.T.);
#820=EDGE_CURVE('',#689,#690,#443,.T.);
#821=EDGE_CURVE('',#690,#690,#602,.T.);
#822=EDGE_CURVE('',#691,#691,#603,.T.);
#823=EDGE_CURVE('',#691,#692,#444,.T.);
#824=EDGE_CURVE('',#692,#692,#604,.T.);
#825=EDGE_CURVE('',#693,#693,#605,.T.);
#826=EDGE_CURVE('',#693,#694,#445,.T.);
#827=EDGE_CURVE('',#694,#694,#606,.T.);
#828=EDGE_CURVE('',#695,#695,#607,.T.);
#829=EDGE_CURVE('',#695,#696,#446,.T.);
#830=EDGE_CURVE('',#696,#696,#608,.T.);
#831=EDGE_CURVE('',#697,#698,#447,.T.);
#832=EDGE_CURVE('',#698,#699,#448,.T.);
#833=EDGE_CURVE('',#699,#700,#449,.T.);
#834=EDGE_CURVE('',#697,#700,#450,.T.);
#835=EDGE_CURVE('',#698,#701,#451,.T.);
#836=EDGE_CURVE('',#701,#702,#452,.T.);
#837=EDGE_CURVE('',#702,#699,#453,.T.);
#838=EDGE_CURVE('',#701,#703,#454,.T.);
#839=EDGE_CURVE('',#703,#704,#455,.T.);
#840=EDGE_CURVE('',#704,#702,#456,.T.);
#841=EDGE_CURVE('',#703,#705,#457,.T.);
#842=EDGE_CURVE('',#705,#706,#458,.T.);
#843=EDGE_CURVE('',#706,#704,#459,.T.);
#844=EDGE_CURVE('',#705,#707,#460,.T.);
#845=EDGE_CURVE('',#707,#708,#461,.T.);
#846=EDGE_CURVE('',#708,#706,#462,.T.);
#847=EDGE_CURVE('',#707,#697,#463,.T.);
#848=EDGE_CURVE('',#700,#708,#464,.T.);
#849=EDGE_CURVE('',#709,#709,#609,.T.);
#850=EDGE_CURVE('',#710,#710,#610,.T.);
#851=EDGE_CURVE('',#710,#709,#465,.T.);
#852=EDGE_CURVE('',#711,#711,#611,.T.);
#853=EDGE_CURVE('',#711,#710,#466,.T.);
#854=EDGE_CURVE('',#711,#712,#467,.T.);
#855=EDGE_CURVE('',#712,#712,#612,.T.);
#856=EDGE_CURVE('',#713,#713,#613,.T.);
#857=EDGE_CURVE('',#713,#714,#468,.T.);
#858=EDGE_CURVE('',#714,#714,#614,.F.);
#859=EDGE_CURVE('',#715,#715,#615,.F.);
#860=EDGE_CURVE('',#715,#714,#469,.T.);
#861=EDGE_CURVE('',#715,#716,#470,.T.);
#862=EDGE_CURVE('',#716,#716,#616,.T.);
#863=EDGE_CURVE('',#717,#717,#617,.T.);
#864=EDGE_CURVE('',#718,#718,#618,.T.);
#865=EDGE_CURVE('',#718,#717,#471,.T.);
#866=ORIENTED_EDGE('',*,*,#719,.F.);
#867=ORIENTED_EDGE('',*,*,#720,.T.);
#868=ORIENTED_EDGE('',*,*,#721,.F.);
#869=ORIENTED_EDGE('',*,*,#720,.F.);
#870=ORIENTED_EDGE('',*,*,#719,.T.);
#871=ORIENTED_EDGE('',*,*,#722,.F.);
#872=ORIENTED_EDGE('',*,*,#723,.T.);
#873=ORIENTED_EDGE('',*,*,#724,.F.);
#874=ORIENTED_EDGE('',*,*,#723,.F.);
#875=ORIENTED_EDGE('',*,*,#722,.T.);
#876=ORIENTED_EDGE('',*,*,#725,.F.);
#877=ORIENTED_EDGE('',*,*,#726,.T.);
#878=ORIENTED_EDGE('',*,*,#727,.F.);
#879=ORIENTED_EDGE('',*,*,#726,.F.);
#880=ORIENTED_EDGE('',*,*,#725,.T.);
#881=ORIENTED_EDGE('',*,*,#728,.F.);
#882=ORIENTED_EDGE('',*,*,#729,.T.);
#883=ORIENTED_EDGE('',*,*,#730,.F.);
#884=ORIENTED_EDGE('',*,*,#729,.F.);
#885=ORIENTED_EDGE('',*,*,#728,.T.);
#886=ORIENTED_EDGE('',*,*,#731,.T.);
#887=ORIENTED_EDGE('',*,*,#732,.T.);
#888=ORIENTED_EDGE('',*,*,#733,.F.);
#889=ORIENTED_EDGE('',*,*,#734,.F.);
#890=ORIENTED_EDGE('',*,*,#735,.T.);
#891=ORIENTED_EDGE('',*,*,#734,.T.);
#892=ORIENTED_EDGE('',*,*,#736,.F.);
#893=ORIENTED_EDGE('',*,*,#737,.F.);
#894=ORIENTED_EDGE('',*,*,#738,.T.);
#895=ORIENTED_EDGE('',*,*,#737,.T.);
#896=ORIENTED_EDGE('',*,*,#739,.F.);
#897=ORIENTED_EDGE('',*,*,#740,.F.);
#898=ORIENTED_EDGE('',*,*,#741,.T.);
#899=ORIENTED_EDGE('',*,*,#740,.T.);
#900=ORIENTED_EDGE('',*,*,#742,.F.);
#901=ORIENTED_EDGE('',*,*,#732,.F.);
#902=ORIENTED_EDGE('',*,*,#742,.T.);
#903=ORIENTED_EDGE('',*,*,#739,.T.);
#904=ORIENTED_EDGE('',*,*,#736,.T.);
#905=ORIENTED_EDGE('',*,*,#733,.T.);
#906=ORIENTED_EDGE('',*,*,#721,.T.);
#907=ORIENTED_EDGE('',*,*,#724,.T.);
#908=ORIENTED_EDGE('',*,*,#727,.T.);
#909=ORIENTED_EDGE('',*,*,#730,.T.);
#910=ORIENTED_EDGE('',*,*,#741,.F.);
#911=ORIENTED_EDGE('',*,*,#731,.F.);
#912=ORIENTED_EDGE('',*,*,#735,.F.);
#913=ORIENTED_EDGE('',*,*,#738,.F.);
#914=ORIENTED_EDGE('',*,*,#743,.F.);
#915=ORIENTED_EDGE('',*,*,#744,.T.);
#916=ORIENTED_EDGE('',*,*,#745,.F.);
#917=ORIENTED_EDGE('',*,*,#744,.F.);
#918=ORIENTED_EDGE('',*,*,#746,.F.);
#919=ORIENTED_EDGE('',*,*,#747,.T.);
#920=ORIENTED_EDGE('',*,*,#748,.F.);
#921=ORIENTED_EDGE('',*,*,#747,.F.);
#922=ORIENTED_EDGE('',*,*,#749,.T.);
#923=ORIENTED_EDGE('',*,*,#749,.F.);
#924=ORIENTED_EDGE('',*,*,#746,.T.);
#925=ORIENTED_EDGE('',*,*,#745,.T.);
#926=ORIENTED_EDGE('',*,*,#750,.F.);
#927=ORIENTED_EDGE('',*,*,#751,.T.);
#928=ORIENTED_EDGE('',*,*,#752,.F.);
#929=ORIENTED_EDGE('',*,*,#753,.F.);
#930=ORIENTED_EDGE('',*,*,#754,.F.);
#931=ORIENTED_EDGE('',*,*,#755,.T.);
#932=ORIENTED_EDGE('',*,*,#756,.F.);
#933=ORIENTED_EDGE('',*,*,#757,.F.);
#934=ORIENTED_EDGE('',*,*,#758,.T.);
#935=ORIENTED_EDGE('',*,*,#759,.F.);
#936=ORIENTED_EDGE('',*,*,#758,.F.);
#937=ORIENTED_EDGE('',*,*,#760,.F.);
#938=ORIENTED_EDGE('',*,*,#751,.F.);
#939=ORIENTED_EDGE('',*,*,#761,.F.);
#940=ORIENTED_EDGE('',*,*,#762,.T.);
#941=ORIENTED_EDGE('',*,*,#763,.F.);
#942=ORIENTED_EDGE('',*,*,#764,.F.);
#943=ORIENTED_EDGE('',*,*,#755,.F.);
#944=ORIENTED_EDGE('',*,*,#765,.F.);
#945=ORIENTED_EDGE('',*,*,#762,.F.);
#946=ORIENTED_EDGE('',*,*,#766,.T.);
#947=ORIENTED_EDGE('',*,*,#767,.T.);
#948=ORIENTED_EDGE('',*,*,#768,.T.);
#949=ORIENTED_EDGE('',*,*,#769,.T.);
#950=ORIENTED_EDGE('',*,*,#770,.T.);
#951=ORIENTED_EDGE('',*,*,#771,.T.);
#952=ORIENTED_EDGE('',*,*,#753,.T.);
#953=ORIENTED_EDGE('',*,*,#764,.T.);
#954=ORIENTED_EDGE('',*,*,#761,.T.);
#955=ORIENTED_EDGE('',*,*,#772,.T.);
#956=ORIENTED_EDGE('',*,*,#773,.T.);
#957=ORIENTED_EDGE('',*,*,#774,.T.);
#958=ORIENTED_EDGE('',*,*,#756,.T.);
#959=ORIENTED_EDGE('',*,*,#759,.T.);
#960=ORIENTED_EDGE('',*,*,#750,.T.);
#961=ORIENTED_EDGE('',*,*,#775,.T.);
#962=ORIENTED_EDGE('',*,*,#776,.T.);
#963=ORIENTED_EDGE('',*,*,#777,.T.);
#964=ORIENTED_EDGE('',*,*,#754,.T.);
#965=ORIENTED_EDGE('',*,*,#777,.F.);
#966=ORIENTED_EDGE('',*,*,#778,.F.);
#967=ORIENTED_EDGE('',*,*,#775,.F.);
#968=ORIENTED_EDGE('',*,*,#752,.T.);
#969=ORIENTED_EDGE('',*,*,#760,.T.);
#970=ORIENTED_EDGE('',*,*,#757,.T.);
#971=ORIENTED_EDGE('',*,*,#774,.F.);
#972=ORIENTED_EDGE('',*,*,#779,.F.);
#973=ORIENTED_EDGE('',*,*,#772,.F.);
#974=ORIENTED_EDGE('',*,*,#763,.T.);
#975=ORIENTED_EDGE('',*,*,#765,.T.);
#976=ORIENTED_EDGE('',*,*,#773,.F.);
#977=ORIENTED_EDGE('',*,*,#779,.T.);
#978=ORIENTED_EDGE('',*,*,#743,.T.);
#979=ORIENTED_EDGE('',*,*,#776,.F.);
#980=ORIENTED_EDGE('',*,*,#778,.T.);
#981=ORIENTED_EDGE('',*,*,#748,.T.);
#982=ORIENTED_EDGE('',*,*,#780,.F.);
#983=ORIENTED_EDGE('',*,*,#781,.T.);
#984=ORIENTED_EDGE('',*,*,#782,.T.);
#985=ORIENTED_EDGE('',*,*,#783,.F.);
#986=ORIENTED_EDGE('',*,*,#784,.F.);
#987=ORIENTED_EDGE('',*,*,#785,.T.);
#988=ORIENTED_EDGE('',*,*,#786,.T.);
#989=ORIENTED_EDGE('',*,*,#781,.F.);
#990=ORIENTED_EDGE('',*,*,#787,.F.);
#991=ORIENTED_EDGE('',*,*,#788,.T.);
#992=ORIENTED_EDGE('',*,*,#789,.T.);
#993=ORIENTED_EDGE('',*,*,#785,.F.);
#994=ORIENTED_EDGE('',*,*,#790,.F.);
#995=ORIENTED_EDGE('',*,*,#783,.T.);
#996=ORIENTED_EDGE('',*,*,#791,.T.);
#997=ORIENTED_EDGE('',*,*,#788,.F.);
#998=ORIENTED_EDGE('',*,*,#791,.F.);
#999=ORIENTED_EDGE('',*,*,#782,.F.);
#1000=ORIENTED_EDGE('',*,*,#786,.F.);
#1001=ORIENTED_EDGE('',*,*,#789,.F.);
#1002=ORIENTED_EDGE('',*,*,#792,.F.);
#1003=ORIENTED_EDGE('',*,*,#793,.T.);
#1004=ORIENTED_EDGE('',*,*,#771,.F.);
#1005=ORIENTED_EDGE('',*,*,#793,.F.);
#1006=ORIENTED_EDGE('',*,*,#794,.F.);
#1007=ORIENTED_EDGE('',*,*,#795,.T.);
#1008=ORIENTED_EDGE('',*,*,#770,.F.);
#1009=ORIENTED_EDGE('',*,*,#795,.F.);
#1010=ORIENTED_EDGE('',*,*,#796,.T.);
#1011=ORIENTED_EDGE('',*,*,#797,.T.);
#1012=ORIENTED_EDGE('',*,*,#769,.F.);
#1013=ORIENTED_EDGE('',*,*,#798,.F.);
#1014=ORIENTED_EDGE('',*,*,#799,.T.);
#1015=ORIENTED_EDGE('',*,*,#798,.T.);
#1016=ORIENTED_EDGE('',*,*,#768,.F.);
#1017=ORIENTED_EDGE('',*,*,#800,.F.);
#1018=ORIENTED_EDGE('',*,*,#801,.T.);
#1019=ORIENTED_EDGE('',*,*,#800,.T.);
#1020=ORIENTED_EDGE('',*,*,#767,.F.);
#1021=ORIENTED_EDGE('',*,*,#802,.F.);
#1022=ORIENTED_EDGE('',*,*,#803,.T.);
#1023=ORIENTED_EDGE('',*,*,#802,.T.);
#1024=ORIENTED_EDGE('',*,*,#766,.F.);
#1025=ORIENTED_EDGE('',*,*,#797,.F.);
#1026=ORIENTED_EDGE('',*,*,#803,.F.);
#1027=ORIENTED_EDGE('',*,*,#796,.F.);
#1028=ORIENTED_EDGE('',*,*,#799,.F.);
#1029=ORIENTED_EDGE('',*,*,#801,.F.);
#1030=ORIENTED_EDGE('',*,*,#780,.T.);
#1031=ORIENTED_EDGE('',*,*,#790,.T.);
#1032=ORIENTED_EDGE('',*,*,#787,.T.);
#1033=ORIENTED_EDGE('',*,*,#784,.T.);
#1034=ORIENTED_EDGE('',*,*,#792,.T.);
#1035=ORIENTED_EDGE('',*,*,#794,.T.);
#1036=ORIENTED_EDGE('',*,*,#804,.F.);
#1037=ORIENTED_EDGE('',*,*,#805,.T.);
#1038=ORIENTED_EDGE('',*,*,#806,.T.);
#1039=ORIENTED_EDGE('',*,*,#805,.F.);
#1040=ORIENTED_EDGE('',*,*,#807,.F.);
#1041=ORIENTED_EDGE('',*,*,#804,.T.);
#1042=ORIENTED_EDGE('',*,*,#808,.T.);
#1043=ORIENTED_EDGE('',*,*,#808,.F.);
#1044=ORIENTED_EDGE('',*,*,#807,.T.);
#1045=ORIENTED_EDGE('',*,*,#809,.F.);
#1046=ORIENTED_EDGE('',*,*,#809,.T.);
#1047=ORIENTED_EDGE('',*,*,#806,.F.);
#1048=ORIENTED_EDGE('',*,*,#810,.F.);
#1049=ORIENTED_EDGE('',*,*,#811,.T.);
#1050=ORIENTED_EDGE('',*,*,#812,.T.);
#1051=ORIENTED_EDGE('',*,*,#811,.F.);
#1052=ORIENTED_EDGE('',*,*,#812,.F.);
#1053=ORIENTED_EDGE('',*,*,#813,.T.);
#1054=ORIENTED_EDGE('',*,*,#814,.F.);
#1055=ORIENTED_EDGE('',*,*,#810,.T.);
#1056=ORIENTED_EDGE('',*,*,#815,.F.);
#1057=ORIENTED_EDGE('',*,*,#816,.T.);
#1058=ORIENTED_EDGE('',*,*,#814,.T.);
#1059=ORIENTED_EDGE('',*,*,#816,.F.);
#1060=ORIENTED_EDGE('',*,*,#815,.T.);
#1061=ORIENTED_EDGE('',*,*,#817,.F.);
#1062=ORIENTED_EDGE('',*,*,#813,.F.);
#1063=ORIENTED_EDGE('',*,*,#818,.T.);
#1064=ORIENTED_EDGE('',*,*,#817,.T.);
#1065=ORIENTED_EDGE('',*,*,#818,.F.);
#1066=ORIENTED_EDGE('',*,*,#819,.T.);
#1067=ORIENTED_EDGE('',*,*,#820,.T.);
#1068=ORIENTED_EDGE('',*,*,#821,.F.);
#1069=ORIENTED_EDGE('',*,*,#820,.F.);
#1070=ORIENTED_EDGE('',*,*,#822,.F.);
#1071=ORIENTED_EDGE('',*,*,#823,.T.);
#1072=ORIENTED_EDGE('',*,*,#824,.T.);
#1073=ORIENTED_EDGE('',*,*,#823,.F.);
#1074=ORIENTED_EDGE('',*,*,#822,.T.);
#1075=ORIENTED_EDGE('',*,*,#821,.T.);
#1076=ORIENTED_EDGE('',*,*,#824,.F.);
#1077=ORIENTED_EDGE('',*,*,#819,.F.);
#1078=ORIENTED_EDGE('',*,*,#825,.T.);
#1079=ORIENTED_EDGE('',*,*,#826,.T.);
#1080=ORIENTED_EDGE('',*,*,#827,.F.);
#1081=ORIENTED_EDGE('',*,*,#826,.F.);
#1082=ORIENTED_EDGE('',*,*,#828,.F.);
#1083=ORIENTED_EDGE('',*,*,#829,.T.);
#1084=ORIENTED_EDGE('',*,*,#830,.T.);
#1085=ORIENTED_EDGE('',*,*,#829,.F.);
#1086=ORIENTED_EDGE('',*,*,#828,.T.);
#1087=ORIENTED_EDGE('',*,*,#827,.T.);
#1088=ORIENTED_EDGE('',*,*,#830,.F.);
#1089=ORIENTED_EDGE('',*,*,#825,.F.);
#1090=ORIENTED_EDGE('',*,*,#831,.T.);
#1091=ORIENTED_EDGE('',*,*,#832,.T.);
#1092=ORIENTED_EDGE('',*,*,#833,.T.);
#1093=ORIENTED_EDGE('',*,*,#834,.F.);
#1094=ORIENTED_EDGE('',*,*,#835,.T.);
#1095=ORIENTED_EDGE('',*,*,#836,.T.);
#1096=ORIENTED_EDGE('',*,*,#837,.T.);
#1097=ORIENTED_EDGE('',*,*,#832,.F.);
#1098=ORIENTED_EDGE('',*,*,#838,.T.);
#1099=ORIENTED_EDGE('',*,*,#839,.T.);
#1100=ORIENTED_EDGE('',*,*,#840,.T.);
#1101=ORIENTED_EDGE('',*,*,#836,.F.);
#1102=ORIENTED_EDGE('',*,*,#841,.T.);
#1103=ORIENTED_EDGE('',*,*,#842,.T.);
#1104=ORIENTED_EDGE('',*,*,#843,.T.);
#1105=ORIENTED_EDGE('',*,*,#839,.F.);
#1106=ORIENTED_EDGE('',*,*,#844,.T.);
#1107=ORIENTED_EDGE('',*,*,#845,.T.);
#1108=ORIENTED_EDGE('',*,*,#846,.T.);
#1109=ORIENTED_EDGE('',*,*,#842,.F.);
#1110=ORIENTED_EDGE('',*,*,#847,.T.);
#1111=ORIENTED_EDGE('',*,*,#834,.T.);
#1112=ORIENTED_EDGE('',*,*,#848,.T.);
#1113=ORIENTED_EDGE('',*,*,#845,.F.);
#1114=ORIENTED_EDGE('',*,*,#847,.F.);
#1115=ORIENTED_EDGE('',*,*,#844,.F.);
#1116=ORIENTED_EDGE('',*,*,#841,.F.);
#1117=ORIENTED_EDGE('',*,*,#838,.F.);
#1118=ORIENTED_EDGE('',*,*,#835,.F.);
#1119=ORIENTED_EDGE('',*,*,#831,.F.);
#1120=ORIENTED_EDGE('',*,*,#848,.F.);
#1121=ORIENTED_EDGE('',*,*,#833,.F.);
#1122=ORIENTED_EDGE('',*,*,#837,.F.);
#1123=ORIENTED_EDGE('',*,*,#840,.F.);
#1124=ORIENTED_EDGE('',*,*,#843,.F.);
#1125=ORIENTED_EDGE('',*,*,#846,.F.);
#1126=ORIENTED_EDGE('',*,*,#849,.F.);
#1127=ORIENTED_EDGE('',*,*,#850,.F.);
#1128=ORIENTED_EDGE('',*,*,#851,.T.);
#1129=ORIENTED_EDGE('',*,*,#849,.T.);
#1130=ORIENTED_EDGE('',*,*,#851,.F.);
#1131=ORIENTED_EDGE('',*,*,#852,.F.);
#1132=ORIENTED_EDGE('',*,*,#853,.T.);
#1133=ORIENTED_EDGE('',*,*,#850,.T.);
#1134=ORIENTED_EDGE('',*,*,#853,.F.);
#1135=ORIENTED_EDGE('',*,*,#852,.T.);
#1136=ORIENTED_EDGE('',*,*,#854,.T.);
#1137=ORIENTED_EDGE('',*,*,#855,.F.);
#1138=ORIENTED_EDGE('',*,*,#854,.F.);
#1139=ORIENTED_EDGE('',*,*,#855,.T.);
#1140=ORIENTED_EDGE('',*,*,#856,.F.);
#1141=ORIENTED_EDGE('',*,*,#856,.T.);
#1142=ORIENTED_EDGE('',*,*,#857,.T.);
#1143=ORIENTED_EDGE('',*,*,#858,.F.);
#1144=ORIENTED_EDGE('',*,*,#857,.F.);
#1145=ORIENTED_EDGE('',*,*,#859,.F.);
#1146=ORIENTED_EDGE('',*,*,#860,.T.);
#1147=ORIENTED_EDGE('',*,*,#858,.T.);
#1148=ORIENTED_EDGE('',*,*,#860,.F.);
#1149=ORIENTED_EDGE('',*,*,#859,.T.);
#1150=ORIENTED_EDGE('',*,*,#861,.T.);
#1151=ORIENTED_EDGE('',*,*,#862,.F.);
#1152=ORIENTED_EDGE('',*,*,#861,.F.);
#1153=ORIENTED_EDGE('',*,*,#862,.T.);
#1154=ORIENTED_EDGE('',*,*,#863,.T.);
#1155=ORIENTED_EDGE('',*,*,#864,.F.);
#1156=ORIENTED_EDGE('',*,*,#865,.T.);
#1157=ORIENTED_EDGE('',*,*,#863,.F.);
#1158=ORIENTED_EDGE('',*,*,#865,.F.);
#1159=ORIENTED_EDGE('',*,*,#864,.T.);
#1160=CYLINDRICAL_SURFACE('',#1346,0.34);
#1161=CYLINDRICAL_SURFACE('',#1350,0.34);
#1162=CYLINDRICAL_SURFACE('',#1354,0.34);
#1163=CYLINDRICAL_SURFACE('',#1358,0.34);
#1164=CYLINDRICAL_SURFACE('',#1370,2.05);
#1165=CYLINDRICAL_SURFACE('',#1373,2.05);
#1166=CYLINDRICAL_SURFACE('',#1391,2.8);
#1167=CYLINDRICAL_SURFACE('',#1401,0.65);
#1168=CYLINDRICAL_SURFACE('',#1403,0.65);
#1169=CYLINDRICAL_SURFACE('',#1411,1.8);
#1170=CYLINDRICAL_SURFACE('',#1420,1.65);
#1171=CYLINDRICAL_SURFACE('',#1427,1.75);
#1172=CYLINDRICAL_SURFACE('',#1431,1.);
#1173=CYLINDRICAL_SURFACE('',#1435,0.425);
#1174=CYLINDRICAL_SURFACE('',#1438,0.645);
#1175=CYLINDRICAL_SURFACE('',#1444,0.42);
#1176=CYLINDRICAL_SURFACE('',#1447,0.8);
#1177=CYLINDRICAL_SURFACE('',#1465,0.65);
#1178=CYLINDRICAL_SURFACE('',#1473,0.3933);
#1179=CYLINDRICAL_SURFACE('',#1481,1.);
#1180=ADVANCED_FACE('',(#197),#1160,.F.);
#1181=ADVANCED_FACE('',(#198),#146,.T.);
#1182=ADVANCED_FACE('',(#199),#1161,.F.);
#1183=ADVANCED_FACE('',(#200),#147,.T.);
#1184=ADVANCED_FACE('',(#201),#1162,.F.);
#1185=ADVANCED_FACE('',(#202),#148,.T.);
#1186=ADVANCED_FACE('',(#203),#1163,.F.);
#1187=ADVANCED_FACE('',(#204),#149,.T.);
#1188=ADVANCED_FACE('',(#205),#150,.T.);
#1189=ADVANCED_FACE('',(#206),#151,.T.);
#1190=ADVANCED_FACE('',(#207),#152,.T.);
#1191=ADVANCED_FACE('',(#208),#153,.T.);
#1192=ADVANCED_FACE('',(#209,#120,#121,#122,#123),#154,.T.);
#1193=ADVANCED_FACE('',(#210),#155,.F.);
#1194=ADVANCED_FACE('',(#211),#1164,.F.);
#1195=ADVANCED_FACE('',(#212),#1165,.F.);
#1196=ADVANCED_FACE('',(#213,#124,#125),#89,.F.);
#1197=ADVANCED_FACE('',(#214),#156,.T.);
#1198=ADVANCED_FACE('',(#215),#157,.T.);
#1199=ADVANCED_FACE('',(#216),#158,.T.);
#1200=ADVANCED_FACE('',(#217),#159,.T.);
#1201=ADVANCED_FACE('',(#218),#160,.T.);
#1202=ADVANCED_FACE('',(#219),#161,.T.);
#1203=ADVANCED_FACE('',(#220,#126,#127,#128),#162,.T.);
#1204=ADVANCED_FACE('',(#221),#1166,.T.);
#1205=ADVANCED_FACE('',(#222,#129),#163,.F.);
#1206=ADVANCED_FACE('',(#223,#130),#164,.T.);
#1207=ADVANCED_FACE('',(#224),#165,.F.);
#1208=ADVANCED_FACE('',(#225),#166,.F.);
#1209=ADVANCED_FACE('',(#226),#167,.F.);
#1210=ADVANCED_FACE('',(#227),#168,.F.);
#1211=ADVANCED_FACE('',(#228),#169,.F.);
#1212=ADVANCED_FACE('',(#229),#1167,.F.);
#1213=ADVANCED_FACE('',(#230),#1168,.F.);
#1214=ADVANCED_FACE('',(#231),#170,.T.);
#1215=ADVANCED_FACE('',(#232),#171,.T.);
#1216=ADVANCED_FACE('',(#233),#172,.T.);
#1217=ADVANCED_FACE('',(#234),#173,.T.);
#1218=ADVANCED_FACE('',(#235,#131,#132,#133),#174,.F.);
#1219=ADVANCED_FACE('',(#236),#1169,.F.);
#1220=ADVANCED_FACE('',(#237,#134),#175,.T.);
#1221=ADVANCED_FACE('',(#238,#135,#136),#90,.T.);
#1222=ADVANCED_FACE('',(#239,#137),#176,.T.);
#1223=ADVANCED_FACE('',(#240),#1170,.T.);
#1224=ADVANCED_FACE('',(#241,#138),#177,.T.);
#1225=ADVANCED_FACE('',(#242,#139),#178,.T.);
#1226=ADVANCED_FACE('',(#243),#1171,.T.);
#1227=ADVANCED_FACE('',(#244,#140),#179,.T.);
#1228=ADVANCED_FACE('',(#245),#1172,.F.);
#1229=ADVANCED_FACE('',(#246),#1173,.F.);
#1230=ADVANCED_FACE('',(#247),#1174,.T.);
#1231=ADVANCED_FACE('',(#248,#141),#180,.T.);
#1232=ADVANCED_FACE('',(#249,#142),#181,.F.);
#1233=ADVANCED_FACE('',(#250),#1175,.F.);
#1234=ADVANCED_FACE('',(#251),#1176,.T.);
#1235=ADVANCED_FACE('',(#252,#143),#182,.T.);
#1236=ADVANCED_FACE('',(#253,#144),#183,.F.);
#1237=ADVANCED_FACE('',(#254),#184,.F.);
#1238=ADVANCED_FACE('',(#255),#185,.F.);
#1239=ADVANCED_FACE('',(#256),#186,.F.);
#1240=ADVANCED_FACE('',(#257),#187,.F.);
#1241=ADVANCED_FACE('',(#258),#188,.F.);
#1242=ADVANCED_FACE('',(#259),#189,.F.);
#1243=ADVANCED_FACE('',(#260),#190,.F.);
#1244=ADVANCED_FACE('',(#261),#191,.F.);
#1245=ADVANCED_FACE('',(#262),#192,.T.);
#1246=ADVANCED_FACE('',(#263),#11,.T.);
#1247=ADVANCED_FACE('',(#264),#1177,.T.);
#1248=ADVANCED_FACE('',(#265),#12,.T.);
#1249=ADVANCED_FACE('',(#266,#145),#193,.T.);
#1250=ADVANCED_FACE('',(#267),#13,.T.);
#1251=ADVANCED_FACE('',(#268),#1178,.T.);
#1252=ADVANCED_FACE('',(#269),#14,.T.);
#1253=ADVANCED_FACE('',(#270),#194,.T.);
#1254=ADVANCED_FACE('',(#271),#195,.F.);
#1255=ADVANCED_FACE('',(#272),#1179,.T.);
#1256=ADVANCED_FACE('',(#273),#196,.T.);
#1257=CLOSED_SHELL('',(#1180,#1181,#1182,#1183,#1184,#1185,#1186,#1187,
#1188,#1189,#1190,#1191,#1192,#1193));
#1258=CLOSED_SHELL('',(#1194,#1195,#1196,#1197,#1198,#1199,#1200,#1201,
#1202,#1203,#1204,#1205,#1206,#1207,#1208,#1209,#1210,#1211,#1212,#1213,
#1214,#1215,#1216,#1217,#1218));
#1259=CLOSED_SHELL('',(#1219,#1220,#1221,#1222));
#1260=CLOSED_SHELL('',(#1223,#1224,#1225,#1226,#1227,#1228));
#1261=CLOSED_SHELL('',(#1229,#1230,#1231,#1232));
#1262=CLOSED_SHELL('',(#1233,#1234,#1235,#1236));
#1263=CLOSED_SHELL('',(#1237,#1238,#1239,#1240,#1241,#1242,#1243,#1244));
#1264=CLOSED_SHELL('',(#1245,#1246,#1247,#1248,#1249,#1250,#1251,#1252,
#1253));
#1265=CLOSED_SHELL('',(#1254,#1255,#1256));
#1266=DERIVED_UNIT_ELEMENT(#1280,1.);
#1267=DERIVED_UNIT_ELEMENT(#2279,-3.);
#1268=DERIVED_UNIT_ELEMENT(#1280,1.);
#1269=DERIVED_UNIT_ELEMENT(#2279,-3.);
#1270=DERIVED_UNIT_ELEMENT(#1280,1.);
#1271=DERIVED_UNIT_ELEMENT(#2279,-3.);
#1272=DERIVED_UNIT_ELEMENT(#1280,1.);
#1273=DERIVED_UNIT_ELEMENT(#2279,-3.);
#1274=DERIVED_UNIT_ELEMENT(#1280,1.);
#1275=DERIVED_UNIT_ELEMENT(#2279,-3.);
#1276=DERIVED_UNIT_ELEMENT(#1280,1.);
#1277=DERIVED_UNIT_ELEMENT(#2279,-3.);
#1278=DERIVED_UNIT_ELEMENT(#1280,1.);
#1279=DERIVED_UNIT_ELEMENT(#2279,-3.);
#1280=(
MASS_UNIT()
NAMED_UNIT(*)
SI_UNIT(.KILO.,.GRAM.)
);
#1281=DERIVED_UNIT((#1266,#1267));
#1282=DERIVED_UNIT((#1268,#1269));
#1283=DERIVED_UNIT((#1270,#1271));
#1284=DERIVED_UNIT((#1272,#1273));
#1285=DERIVED_UNIT((#1274,#1275));
#1286=DERIVED_UNIT((#1276,#1277));
#1287=DERIVED_UNIT((#1278,#1279));
#1288=MEASURE_REPRESENTATION_ITEM('density measure',
POSITIVE_RATIO_MEASURE(7850.),#1281);
#1289=MEASURE_REPRESENTATION_ITEM('density measure',
POSITIVE_RATIO_MEASURE(7850.),#1282);
#1290=MEASURE_REPRESENTATION_ITEM('density measure',
POSITIVE_RATIO_MEASURE(7850.),#1283);
#1291=MEASURE_REPRESENTATION_ITEM('density measure',
POSITIVE_RATIO_MEASURE(7850.),#1284);
#1292=MEASURE_REPRESENTATION_ITEM('density measure',
POSITIVE_RATIO_MEASURE(7850.),#1285);
#1293=MEASURE_REPRESENTATION_ITEM('density measure',
POSITIVE_RATIO_MEASURE(7850.),#1286);
#1294=MEASURE_REPRESENTATION_ITEM('density measure',
POSITIVE_RATIO_MEASURE(7850.),#1287);
#1295=PROPERTY_DEFINITION_REPRESENTATION(#1330,#1309);
#1296=PROPERTY_DEFINITION_REPRESENTATION(#1331,#1310);
#1297=PROPERTY_DEFINITION_REPRESENTATION(#1332,#1311);
#1298=PROPERTY_DEFINITION_REPRESENTATION(#1333,#1312);
#1299=PROPERTY_DEFINITION_REPRESENTATION(#1334,#1313);
#1300=PROPERTY_DEFINITION_REPRESENTATION(#1335,#1314);
#1301=PROPERTY_DEFINITION_REPRESENTATION(#1336,#1315);
#1302=PROPERTY_DEFINITION_REPRESENTATION(#1337,#1316);
#1303=PROPERTY_DEFINITION_REPRESENTATION(#1338,#1317);
#1304=PROPERTY_DEFINITION_REPRESENTATION(#1339,#1318);
#1305=PROPERTY_DEFINITION_REPRESENTATION(#1340,#1319);
#1306=PROPERTY_DEFINITION_REPRESENTATION(#1341,#1320);
#1307=PROPERTY_DEFINITION_REPRESENTATION(#1342,#1321);
#1308=PROPERTY_DEFINITION_REPRESENTATION(#1343,#1322);
#1309=REPRESENTATION('material name',(#1323),#2269);
#1310=REPRESENTATION('density',(#1288),#2269);
#1311=REPRESENTATION('material name',(#1324),#2271);
#1312=REPRESENTATION('density',(#1289),#2271);
#1313=REPRESENTATION('material name',(#1325),#2272);
#1314=REPRESENTATION('density',(#1290),#2272);
#1315=REPRESENTATION('material name',(#1326),#2273);
#1316=REPRESENTATION('density',(#1291),#2273);
#1317=REPRESENTATION('material name',(#1327),#2274);
#1318=REPRESENTATION('density',(#1292),#2274);
#1319=REPRESENTATION('material name',(#1328),#2275);
#1320=REPRESENTATION('density',(#1293),#2275);
#1321=REPRESENTATION('material name',(#1329),#2276);
#1322=REPRESENTATION('density',(#1294),#2276);
#1323=DESCRIPTIVE_REPRESENTATION_ITEM('Steel','Steel');
#1324=DESCRIPTIVE_REPRESENTATION_ITEM('Steel','Steel');
#1325=DESCRIPTIVE_REPRESENTATION_ITEM('Steel','Steel');
#1326=DESCRIPTIVE_REPRESENTATION_ITEM('Steel','Steel');
#1327=DESCRIPTIVE_REPRESENTATION_ITEM('Steel','Steel');
#1328=DESCRIPTIVE_REPRESENTATION_ITEM('Steel','Steel');
#1329=DESCRIPTIVE_REPRESENTATION_ITEM('Steel','Steel');
#1330=PROPERTY_DEFINITION('material property','material name',#2329);
#1331=PROPERTY_DEFINITION('material property','density of part',#2329);
#1332=PROPERTY_DEFINITION('material property','material name',#2331);
#1333=PROPERTY_DEFINITION('material property','density of part',#2331);
#1334=PROPERTY_DEFINITION('material property','material name',#2332);
#1335=PROPERTY_DEFINITION('material property','density of part',#2332);
#1336=PROPERTY_DEFINITION('material property','material name',#2333);
#1337=PROPERTY_DEFINITION('material property','density of part',#2333);
#1338=PROPERTY_DEFINITION('material property','material name',#2334);
#1339=PROPERTY_DEFINITION('material property','density of part',#2334);
#1340=PROPERTY_DEFINITION('material property','material name',#2335);
#1341=PROPERTY_DEFINITION('material property','density of part',#2335);
#1342=PROPERTY_DEFINITION('material property','material name',#2336);
#1343=PROPERTY_DEFINITION('material property','density of part',#2336);
#1344=AXIS2_PLACEMENT_3D('',#1907,#1500,#1501);
#1345=AXIS2_PLACEMENT_3D('',#1908,#1502,#1503);
#1346=AXIS2_PLACEMENT_3D('',#1909,#1504,#1505);
#1347=AXIS2_PLACEMENT_3D('',#1911,#1506,#1507);
#1348=AXIS2_PLACEMENT_3D('',#1914,#1509,#1510);
#1349=AXIS2_PLACEMENT_3D('',#1915,#1511,#1512);
#1350=AXIS2_PLACEMENT_3D('',#1916,#1513,#1514);
#1351=AXIS2_PLACEMENT_3D('',#1918,#1515,#1516);
#1352=AXIS2_PLACEMENT_3D('',#1921,#1518,#1519);
#1353=AXIS2_PLACEMENT_3D('',#1922,#1520,#1521);
#1354=AXIS2_PLACEMENT_3D('',#1923,#1522,#1523);
#1355=AXIS2_PLACEMENT_3D('',#1925,#1524,#1525);
#1356=AXIS2_PLACEMENT_3D('',#1928,#1527,#1528);
#1357=AXIS2_PLACEMENT_3D('',#1929,#1529,#1530);
#1358=AXIS2_PLACEMENT_3D('',#1930,#1531,#1532);
#1359=AXIS2_PLACEMENT_3D('',#1932,#1533,#1534);
#1360=AXIS2_PLACEMENT_3D('',#1935,#1536,#1537);
#1361=AXIS2_PLACEMENT_3D('',#1936,#1538,#1539);
#1362=AXIS2_PLACEMENT_3D('',#1937,#1540,#1541);
#1363=AXIS2_PLACEMENT_3D('',#1946,#1546,#1547);
#1364=AXIS2_PLACEMENT_3D('',#1952,#1551,#1552);
#1365=AXIS2_PLACEMENT_3D('',#1958,#1556,#1557);
#1366=AXIS2_PLACEMENT_3D('',#1961,#1560,#1561);
#1367=AXIS2_PLACEMENT_3D('',#1962,#1562,#1563);
#1368=AXIS2_PLACEMENT_3D('',#1963,#1564,#1565);
#1369=AXIS2_PLACEMENT_3D('',#1964,#1566,#1567);
#1370=AXIS2_PLACEMENT_3D('',#1965,#1568,#1569);
#1371=AXIS2_PLACEMENT_3D('',#1967,#1570,#1571);
#1372=AXIS2_PLACEMENT_3D('',#1970,#1573,#1574);
#1373=AXIS2_PLACEMENT_3D('',#1971,#1575,#1576);
#1374=AXIS2_PLACEMENT_3D('',#1973,#1577,#1578);
#1375=AXIS2_PLACEMENT_3D('',#1976,#1580,#1581);
#1376=AXIS2_PLACEMENT_3D('',#1977,#1582,#1583);
#1377=AXIS2_PLACEMENT_3D('',#1980,#1584,#1585);
#1378=AXIS2_PLACEMENT_3D('',#1981,#1586,#1587);
#1379=AXIS2_PLACEMENT_3D('',#1987,#1590,#1591);
#1380=AXIS2_PLACEMENT_3D('',#1988,#1592,#1593);
#1381=AXIS2_PLACEMENT_3D('',#1993,#1595,#1596);
#1382=AXIS2_PLACEMENT_3D('',#1995,#1598,#1599);
#1383=AXIS2_PLACEMENT_3D('',#2000,#1601,#1602);
#1384=AXIS2_PLACEMENT_3D('',#2002,#1604,#1605);
#1385=AXIS2_PLACEMENT_3D('',#2005,#1608,#1609);
#1386=AXIS2_PLACEMENT_3D('',#2011,#1612,#1613);
#1387=AXIS2_PLACEMENT_3D('',#2012,#1614,#1615);
#1388=AXIS2_PLACEMENT_3D('',#2015,#1618,#1619);
#1389=AXIS2_PLACEMENT_3D('',#2025,#1624,#1625);
#1390=AXIS2_PLACEMENT_3D('',#2027,#1626,#1627);
#1391=AXIS2_PLACEMENT_3D('',#2038,#1634,#1635);
#1392=AXIS2_PLACEMENT_3D('',#2039,#1636,#1637);
#1393=AXIS2_PLACEMENT_3D('',#2040,#1638,#1639);
#1394=AXIS2_PLACEMENT_3D('',#2041,#1640,#1641);
#1395=AXIS2_PLACEMENT_3D('',#2042,#1642,#1643);
#1396=AXIS2_PLACEMENT_3D('',#2043,#1644,#1645);
#1397=AXIS2_PLACEMENT_3D('',#2052,#1650,#1651);
#1398=AXIS2_PLACEMENT_3D('',#2058,#1655,#1656);
#1399=AXIS2_PLACEMENT_3D('',#2064,#1660,#1661);
#1400=AXIS2_PLACEMENT_3D('',#2067,#1664,#1665);
#1401=AXIS2_PLACEMENT_3D('',#2068,#1666,#1667);
#1402=AXIS2_PLACEMENT_3D('',#2070,#1668,#1669);
#1403=AXIS2_PLACEMENT_3D('',#2072,#1671,#1672);
#1404=AXIS2_PLACEMENT_3D('',#2074,#1673,#1674);
#1405=AXIS2_PLACEMENT_3D('',#2076,#1676,#1677);
#1406=AXIS2_PLACEMENT_3D('',#2082,#1681,#1682);
#1407=AXIS2_PLACEMENT_3D('',#2086,#1685,#1686);
#1408=AXIS2_PLACEMENT_3D('',#2090,#1689,#1690);
#1409=AXIS2_PLACEMENT_3D('',#2092,#1692,#1693);
#1410=AXIS2_PLACEMENT_3D('',#2093,#1694,#1695);
#1411=AXIS2_PLACEMENT_3D('',#2094,#1696,#1697);
#1412=AXIS2_PLACEMENT_3D('',#2096,#1698,#1699);
#1413=AXIS2_PLACEMENT_3D('',#2099,#1701,#1702);
#1414=AXIS2_PLACEMENT_3D('',#2100,#1703,#1704);
#1415=AXIS2_PLACEMENT_3D('',#2102,#1705,#1706);
#1416=AXIS2_PLACEMENT_3D('',#2103,#1707,#1708);
#1417=AXIS2_PLACEMENT_3D('',#2106,#1709,#1710);
#1418=AXIS2_PLACEMENT_3D('',#2108,#1711,#1712);
#1419=AXIS2_PLACEMENT_3D('',#2109,#1713,#1714);
#1420=AXIS2_PLACEMENT_3D('',#2110,#1715,#1716);
#1421=AXIS2_PLACEMENT_3D('',#2112,#1717,#1718);
#1422=AXIS2_PLACEMENT_3D('',#2115,#1720,#1721);
#1423=AXIS2_PLACEMENT_3D('',#2116,#1722,#1723);
#1424=AXIS2_PLACEMENT_3D('',#2118,#1724,#1725);
#1425=AXIS2_PLACEMENT_3D('',#2119,#1726,#1727);
#1426=AXIS2_PLACEMENT_3D('',#2121,#1728,#1729);
#1427=AXIS2_PLACEMENT_3D('',#2122,#1730,#1731);
#1428=AXIS2_PLACEMENT_3D('',#2124,#1732,#1733);
#1429=AXIS2_PLACEMENT_3D('',#2126,#1735,#1736);
#1430=AXIS2_PLACEMENT_3D('',#2128,#1737,#1738);
#1431=AXIS2_PLACEMENT_3D('',#2129,#1739,#1740);
#1432=AXIS2_PLACEMENT_3D('',#2131,#1742,#1743);
#1433=AXIS2_PLACEMENT_3D('',#2132,#1744,#1745);
#1434=AXIS2_PLACEMENT_3D('',#2133,#1746,#1747);
#1435=AXIS2_PLACEMENT_3D('',#2134,#1748,#1749);
#1436=AXIS2_PLACEMENT_3D('',#2136,#1750,#1751);
#1437=AXIS2_PLACEMENT_3D('',#2139,#1753,#1754);
#1438=AXIS2_PLACEMENT_3D('',#2140,#1755,#1756);
#1439=AXIS2_PLACEMENT_3D('',#2142,#1757,#1758);
#1440=AXIS2_PLACEMENT_3D('',#2145,#1760,#1761);
#1441=AXIS2_PLACEMENT_3D('',#2146,#1762,#1763);
#1442=AXIS2_PLACEMENT_3D('',#2147,#1764,#1765);
#1443=AXIS2_PLACEMENT_3D('',#2148,#1766,#1767);
#1444=AXIS2_PLACEMENT_3D('',#2149,#1768,#1769);
#1445=AXIS2_PLACEMENT_3D('',#2151,#1770,#1771);
#1446=AXIS2_PLACEMENT_3D('',#2154,#1773,#1774);
#1447=AXIS2_PLACEMENT_3D('',#2155,#1775,#1776);
#1448=AXIS2_PLACEMENT_3D('',#2157,#1777,#1778);
#1449=AXIS2_PLACEMENT_3D('',#2160,#1780,#1781);
#1450=AXIS2_PLACEMENT_3D('',#2161,#1782,#1783);
#1451=AXIS2_PLACEMENT_3D('',#2162,#1784,#1785);
#1452=AXIS2_PLACEMENT_3D('',#2163,#1786,#1787);
#1453=AXIS2_PLACEMENT_3D('',#2164,#1788,#1789);
#1454=AXIS2_PLACEMENT_3D('',#2173,#1794,#1795);
#1455=AXIS2_PLACEMENT_3D('',#2179,#1799,#1800);
#1456=AXIS2_PLACEMENT_3D('',#2185,#1804,#1805);
#1457=AXIS2_PLACEMENT_3D('',#2191,#1809,#1810);
#1458=AXIS2_PLACEMENT_3D('',#2197,#1814,#1815);
#1459=AXIS2_PLACEMENT_3D('',#2200,#1818,#1819);
#1460=AXIS2_PLACEMENT_3D('',#2201,#1820,#1821);
#1461=AXIS2_PLACEMENT_3D('',#2202,#1822,#1823);
#1462=AXIS2_PLACEMENT_3D('',#2204,#1824,#1825);
#1463=AXIS2_PLACEMENT_3D('',#2205,#1826,#1827);
#1464=AXIS2_PLACEMENT_3D('',#2207,#1828,#1829);
#1465=AXIS2_PLACEMENT_3D('',#2209,#1831,#1832);
#1466=AXIS2_PLACEMENT_3D('',#2211,#1833,#1834);
#1467=AXIS2_PLACEMENT_3D('',#2213,#1836,#1837);
#1468=AXIS2_PLACEMENT_3D('',#2216,#1839,#1840);
#1469=AXIS2_PLACEMENT_3D('',#2217,#1841,#1842);
#1470=AXIS2_PLACEMENT_3D('',#2219,#1843,#1844);
#1471=AXIS2_PLACEMENT_3D('',#2220,#1845,#1846);
#1472=AXIS2_PLACEMENT_3D('',#2223,#1848,#1849);
#1473=AXIS2_PLACEMENT_3D('',#2224,#1850,#1851);
#1474=AXIS2_PLACEMENT_3D('',#2226,#1852,#1853);
#1475=AXIS2_PLACEMENT_3D('',#2228,#1855,#1856);
#1476=AXIS2_PLACEMENT_3D('',#2231,#1858,#1859);
#1477=AXIS2_PLACEMENT_3D('',#2232,#1860,#1861);
#1478=AXIS2_PLACEMENT_3D('',#2233,#1862,#1863);
#1479=AXIS2_PLACEMENT_3D('',#2234,#1864,#1865);
#1480=AXIS2_PLACEMENT_3D('',#2236,#1866,#1867);
#1481=AXIS2_PLACEMENT_3D('',#2237,#1868,#1869);
#1482=AXIS2_PLACEMENT_3D('',#2239,#1870,#1871);
#1483=AXIS2_PLACEMENT_3D('',#2241,#1873,#1874);
#1484=AXIS2_PLACEMENT_3D('',#2242,#1875,#1876);
#1485=AXIS2_PLACEMENT_3D('',#2243,#1877,#1878);
#1486=AXIS2_PLACEMENT_3D('',#2244,#1879,#1880);
#1487=AXIS2_PLACEMENT_3D('',#2245,#1881,#1882);
#1488=AXIS2_PLACEMENT_3D('',#2246,#1883,#1884);
#1489=AXIS2_PLACEMENT_3D('',#2247,#1885,#1886);
#1490=AXIS2_PLACEMENT_3D('',#2248,#1887,#1888);
#1491=AXIS2_PLACEMENT_3D('',#2249,#1889,#1890);
#1492=AXIS2_PLACEMENT_3D('',#2250,#1891,#1892);
#1493=AXIS2_PLACEMENT_3D('',#2251,#1893,#1894);
#1494=AXIS2_PLACEMENT_3D('',#2252,#1895,#1896);
#1495=AXIS2_PLACEMENT_3D('',#2253,#1897,#1898);
#1496=AXIS2_PLACEMENT_3D('',#2254,#1899,#1900);
#1497=AXIS2_PLACEMENT_3D('',#2255,#1901,#1902);
#1498=AXIS2_PLACEMENT_3D('',#2256,#1903,#1904);
#1499=AXIS2_PLACEMENT_3D('',#2257,#1905,#1906);
#1500=DIRECTION('axis',(0.,0.,1.));
#1501=DIRECTION('refdir',(1.,0.,0.));
#1502=DIRECTION('axis',(0.,0.,1.));
#1503=DIRECTION('refdir',(1.,0.,0.));
#1504=DIRECTION('center_axis',(0.,0.,1.));
#1505=DIRECTION('ref_axis',(1.,0.,0.));
#1506=DIRECTION('center_axis',(0.,0.,1.));
#1507=DIRECTION('ref_axis',(1.,0.,0.));
#1508=DIRECTION('',(0.,0.,1.));
#1509=DIRECTION('center_axis',(0.,0.,-1.));
#1510=DIRECTION('ref_axis',(1.,0.,0.));
#1511=DIRECTION('center_axis',(0.,0.,1.));
#1512=DIRECTION('ref_axis',(1.,0.,0.));
#1513=DIRECTION('center_axis',(0.,0.,1.));
#1514=DIRECTION('ref_axis',(1.,0.,0.));
#1515=DIRECTION('center_axis',(0.,0.,1.));
#1516=DIRECTION('ref_axis',(1.,0.,0.));
#1517=DIRECTION('',(0.,0.,1.));
#1518=DIRECTION('center_axis',(0.,0.,-1.));
#1519=DIRECTION('ref_axis',(1.,0.,0.));
#1520=DIRECTION('center_axis',(0.,0.,1.));
#1521=DIRECTION('ref_axis',(1.,0.,0.));
#1522=DIRECTION('center_axis',(0.,0.,1.));
#1523=DIRECTION('ref_axis',(1.,0.,0.));
#1524=DIRECTION('center_axis',(0.,0.,1.));
#1525=DIRECTION('ref_axis',(1.,0.,0.));
#1526=DIRECTION('',(0.,0.,1.));
#1527=DIRECTION('center_axis',(0.,0.,-1.));
#1528=DIRECTION('ref_axis',(1.,0.,0.));
#1529=DIRECTION('center_axis',(0.,0.,1.));
#1530=DIRECTION('ref_axis',(1.,0.,0.));
#1531=DIRECTION('center_axis',(0.,0.,1.));
#1532=DIRECTION('ref_axis',(1.,0.,0.));
#1533=DIRECTION('center_axis',(0.,0.,1.));
#1534=DIRECTION('ref_axis',(1.,0.,0.));
#1535=DIRECTION('',(0.,0.,1.));
#1536=DIRECTION('center_axis',(0.,0.,-1.));
#1537=DIRECTION('ref_axis',(1.,0.,0.));
#1538=DIRECTION('center_axis',(0.,0.,1.));
#1539=DIRECTION('ref_axis',(1.,0.,0.));
#1540=DIRECTION('center_axis',(0.,1.,0.));
#1541=DIRECTION('ref_axis',(-1.,0.,0.));
#1542=DIRECTION('',(-1.,0.,0.));
#1543=DIRECTION('',(0.,0.,1.));
#1544=DIRECTION('',(-1.,0.,0.));
#1545=DIRECTION('',(0.,0.,1.));
#1546=DIRECTION('center_axis',(1.,0.,0.));
#1547=DIRECTION('ref_axis',(0.,1.,0.));
#1548=DIRECTION('',(0.,1.,0.));
#1549=DIRECTION('',(0.,1.,0.));
#1550=DIRECTION('',(0.,0.,1.));
#1551=DIRECTION('center_axis',(0.,-1.,0.));
#1552=DIRECTION('ref_axis',(1.,0.,0.));
#1553=DIRECTION('',(1.,0.,0.));
#1554=DIRECTION('',(1.,0.,0.));
#1555=DIRECTION('',(0.,0.,1.));
#1556=DIRECTION('center_axis',(-1.,0.,0.));
#1557=DIRECTION('ref_axis',(0.,-1.,0.));
#1558=DIRECTION('',(0.,-1.,0.));
#1559=DIRECTION('',(0.,-1.,0.));
#1560=DIRECTION('center_axis',(0.,0.,1.));
#1561=DIRECTION('ref_axis',(1.,0.,0.));
#1562=DIRECTION('center_axis',(0.,0.,1.));
#1563=DIRECTION('ref_axis',(1.,0.,0.));
#1564=DIRECTION('axis',(0.,0.,1.));
#1565=DIRECTION('refdir',(1.,0.,0.));
#1566=DIRECTION('axis',(0.,0.,1.));
#1567=DIRECTION('refdir',(1.,0.,0.));
#1568=DIRECTION('center_axis',(0.,1.,0.));
#1569=DIRECTION('ref_axis',(1.,0.,0.));
#1570=DIRECTION('center_axis',(0.,1.,0.));
#1571=DIRECTION('ref_axis',(1.,0.,0.));
#1572=DIRECTION('',(0.,1.,0.));
#1573=DIRECTION('center_axis',(0.,-1.,0.));
#1574=DIRECTION('ref_axis',(1.,0.,0.));
#1575=DIRECTION('center_axis',(0.,1.,0.));
#1576=DIRECTION('ref_axis',(1.,0.,0.));
#1577=DIRECTION('center_axis',(0.,1.,0.));
#1578=DIRECTION('ref_axis',(1.,0.,0.));
#1579=DIRECTION('',(0.,1.,0.));
#1580=DIRECTION('center_axis',(0.,-1.,0.));
#1581=DIRECTION('ref_axis',(1.,0.,0.));
#1582=DIRECTION('center_axis',(1.22464679914735E-16,0.,1.));
#1583=DIRECTION('ref_axis',(1.,0.,-6.12323399573677E-17));
#1584=DIRECTION('center_axis',(-1.22464679914735E-16,1.,7.49879891330929E-33));
#1585=DIRECTION('ref_axis',(-1.,-1.22464679914735E-16,6.12323399573677E-17));
#1586=DIRECTION('center_axis',(0.,1.,0.));
#1587=DIRECTION('ref_axis',(0.,0.,1.));
#1588=DIRECTION('',(1.,0.,0.));
#1589=DIRECTION('',(0.850265146687862,0.,0.526354614616295));
#1590=DIRECTION('center_axis',(0.,1.,0.));
#1591=DIRECTION('ref_axis',(1.,0.,0.));
#1592=DIRECTION('center_axis',(0.,1.,0.));
#1593=DIRECTION('ref_axis',(0.,0.,1.));
#1594=DIRECTION('',(1.,0.,0.));
#1595=DIRECTION('center_axis',(0.,1.,0.));
#1596=DIRECTION('ref_axis',(1.,0.,0.));
#1597=DIRECTION('',(0.850265146687862,0.,-0.526354614616295));
#1598=DIRECTION('center_axis',(0.,-1.,0.));
#1599=DIRECTION('ref_axis',(0.,0.,-1.));
#1600=DIRECTION('',(-1.,0.,0.));
#1601=DIRECTION('center_axis',(0.,-1.,0.));
#1602=DIRECTION('ref_axis',(1.,0.,0.));
#1603=DIRECTION('',(-0.850265146687862,0.,-0.526354614616295));
#1604=DIRECTION('center_axis',(-0.526354614616295,0.,0.850265146687862));
#1605=DIRECTION('ref_axis',(0.850265146687862,0.,0.526354614616295));
#1606=DIRECTION('',(0.,1.,0.));
#1607=DIRECTION('',(0.,-1.,0.));
#1608=DIRECTION('center_axis',(0.,-1.,0.));
#1609=DIRECTION('ref_axis',(0.,0.,-1.));
#1610=DIRECTION('',(-1.,0.,0.));
#1611=DIRECTION('',(-0.850265146687862,0.,0.526354614616295));
#1612=DIRECTION('center_axis',(0.,-1.,0.));
#1613=DIRECTION('ref_axis',(1.,0.,0.));
#1614=DIRECTION('center_axis',(0.526354614616295,0.,0.850265146687862));
#1615=DIRECTION('ref_axis',(0.850265146687862,0.,-0.526354614616295));
#1616=DIRECTION('',(0.,-1.,0.));
#1617=DIRECTION('',(0.,1.,0.));
#1618=DIRECTION('center_axis',(0.,0.,1.));
#1619=DIRECTION('ref_axis',(1.,0.,0.));
#1620=DIRECTION('',(0.,-1.,0.));
#1621=DIRECTION('',(1.,0.,0.));
#1622=DIRECTION('',(0.,1.,0.));
#1623=DIRECTION('',(-1.,0.,0.));
#1624=DIRECTION('center_axis',(0.,0.,-1.));
#1625=DIRECTION('ref_axis',(1.,0.,0.));
#1626=DIRECTION('center_axis',(0.,0.,-1.));
#1627=DIRECTION('ref_axis',(1.,0.,0.));
#1628=DIRECTION('',(0.,-1.,0.));
#1629=DIRECTION('',(-1.,0.,0.));
#1630=DIRECTION('',(0.,1.,0.));
#1631=DIRECTION('',(0.,1.,0.));
#1632=DIRECTION('',(1.,0.,0.));
#1633=DIRECTION('',(0.,-1.,0.));
#1634=DIRECTION('center_axis',(0.,1.,0.));
#1635=DIRECTION('ref_axis',(6.12323399573677E-17,0.,1.));
#1636=DIRECTION('center_axis',(0.,1.,0.));
#1637=DIRECTION('ref_axis',(1.,0.,0.));
#1638=DIRECTION('center_axis',(0.,-1.,0.));
#1639=DIRECTION('ref_axis',(1.,0.,0.));
#1640=DIRECTION('center_axis',(0.,1.,0.));
#1641=DIRECTION('ref_axis',(1.,0.,0.));
#1642=DIRECTION('center_axis',(0.,1.,0.));
#1643=DIRECTION('ref_axis',(1.,0.,0.));
#1644=DIRECTION('center_axis',(0.,1.,0.));
#1645=DIRECTION('ref_axis',(-1.,0.,0.));
#1646=DIRECTION('',(-1.,0.,0.));
#1647=DIRECTION('',(0.,0.,1.));
#1648=DIRECTION('',(-1.,0.,0.));
#1649=DIRECTION('',(0.,0.,1.));
#1650=DIRECTION('center_axis',(1.,0.,0.));
#1651=DIRECTION('ref_axis',(0.,1.,0.));
#1652=DIRECTION('',(0.,1.,0.));
#1653=DIRECTION('',(0.,0.,1.));
#1654=DIRECTION('',(0.,1.,0.));
#1655=DIRECTION('center_axis',(0.,-1.,0.));
#1656=DIRECTION('ref_axis',(1.,0.,0.));
#1657=DIRECTION('',(1.,0.,0.));
#1658=DIRECTION('',(0.,0.,1.));
#1659=DIRECTION('',(1.,0.,0.));
#1660=DIRECTION('center_axis',(-1.,0.,0.));
#1661=DIRECTION('ref_axis',(0.,-1.,0.));
#1662=DIRECTION('',(0.,-1.,0.));
#1663=DIRECTION('',(0.,-1.,0.));
#1664=DIRECTION('center_axis',(0.,0.,1.));
#1665=DIRECTION('ref_axis',(1.,0.,0.));
#1666=DIRECTION('center_axis',(0.,0.,1.));
#1667=DIRECTION('ref_axis',(1.,0.,0.));
#1668=DIRECTION('center_axis',(0.,0.,1.));
#1669=DIRECTION('ref_axis',(1.,0.,0.));
#1670=DIRECTION('',(0.,0.,1.));
#1671=DIRECTION('center_axis',(0.,0.,1.));
#1672=DIRECTION('ref_axis',(1.,0.,0.));
#1673=DIRECTION('center_axis',(0.,0.,1.));
#1674=DIRECTION('ref_axis',(1.,0.,0.));
#1675=DIRECTION('',(0.,0.,1.));
#1676=DIRECTION('center_axis',(0.,1.,0.));
#1677=DIRECTION('ref_axis',(-1.,0.,0.));
#1678=DIRECTION('',(-1.,0.,0.));
#1679=DIRECTION('',(0.,0.,1.));
#1680=DIRECTION('',(0.,0.,1.));
#1681=DIRECTION('center_axis',(1.,0.,0.));
#1682=DIRECTION('ref_axis',(0.,1.,0.));
#1683=DIRECTION('',(0.,1.,0.));
#1684=DIRECTION('',(0.,0.,1.));
#1685=DIRECTION('center_axis',(0.,-1.,0.));
#1686=DIRECTION('ref_axis',(1.,0.,0.));
#1687=DIRECTION('',(1.,0.,0.));
#1688=DIRECTION('',(0.,0.,1.));
#1689=DIRECTION('center_axis',(-1.,0.,0.));
#1690=DIRECTION('ref_axis',(0.,-1.,0.));
#1691=DIRECTION('',(0.,-1.,0.));
#1692=DIRECTION('center_axis',(0.,0.,1.));
#1693=DIRECTION('ref_axis',(1.,0.,0.));
#1694=DIRECTION('axis',(0.,0.,1.));
#1695=DIRECTION('refdir',(1.,0.,0.));
#1696=DIRECTION('center_axis',(0.,-1.,0.));
#1697=DIRECTION('ref_axis',(1.,0.,0.));
#1698=DIRECTION('center_axis',(0.,-1.,0.));
#1699=DIRECTION('ref_axis',(1.,0.,0.));
#1700=DIRECTION('',(0.,-1.,0.));
#1701=DIRECTION('center_axis',(0.,-1.,0.));
#1702=DIRECTION('ref_axis',(1.,0.,0.));
#1703=DIRECTION('center_axis',(0.,1.,0.));
#1704=DIRECTION('ref_axis',(0.,0.,1.));
#1705=DIRECTION('center_axis',(0.,-1.,0.));
#1706=DIRECTION('ref_axis',(1.,0.,0.));
#1707=DIRECTION('center_axis',(1.22464679914735E-16,0.,1.));
#1708=DIRECTION('ref_axis',(1.,0.,-6.12323399573677E-17));
#1709=DIRECTION('center_axis',(1.22464679914735E-16,-1.,-7.49879891330929E-33));
#1710=DIRECTION('ref_axis',(-1.,-1.22464679914735E-16,6.12323399573677E-17));
#1711=DIRECTION('center_axis',(0.,-1.,0.));
#1712=DIRECTION('ref_axis',(1.,0.,0.));
#1713=DIRECTION('center_axis',(0.,-1.,0.));
#1714=DIRECTION('ref_axis',(0.,0.,-1.));
#1715=DIRECTION('center_axis',(0.,-1.,0.));
#1716=DIRECTION('ref_axis',(1.,0.,0.));
#1717=DIRECTION('center_axis',(0.,-1.,0.));
#1718=DIRECTION('ref_axis',(1.,0.,0.));
#1719=DIRECTION('',(0.,1.,0.));
#1720=DIRECTION('center_axis',(0.,-1.,0.));
#1721=DIRECTION('ref_axis',(1.,0.,0.));
#1722=DIRECTION('center_axis',(0.,1.,0.));
#1723=DIRECTION('ref_axis',(0.,0.,1.));
#1724=DIRECTION('center_axis',(0.,-1.,0.));
#1725=DIRECTION('ref_axis',(1.,0.,0.));
#1726=DIRECTION('center_axis',(0.,1.,0.));
#1727=DIRECTION('ref_axis',(0.,0.,1.));
#1728=DIRECTION('center_axis',(0.,-1.,0.));
#1729=DIRECTION('ref_axis',(1.,0.,0.));
#1730=DIRECTION('center_axis',(0.,-1.,0.));
#1731=DIRECTION('ref_axis',(1.,0.,0.));
#1732=DIRECTION('center_axis',(0.,-1.,0.));
#1733=DIRECTION('ref_axis',(1.,0.,0.));
#1734=DIRECTION('',(0.,1.,0.));
#1735=DIRECTION('center_axis',(0.,-1.,0.));
#1736=DIRECTION('ref_axis',(0.,0.,-1.));
#1737=DIRECTION('center_axis',(0.,-1.,0.));
#1738=DIRECTION('ref_axis',(1.,0.,0.));
#1739=DIRECTION('center_axis',(0.,-1.,0.));
#1740=DIRECTION('ref_axis',(1.,0.,0.));
#1741=DIRECTION('',(0.,-1.,0.));
#1742=DIRECTION('',(0.,0.,1.));
#1743=DIRECTION('',(1.,0.,0.));
#1744=DIRECTION('',(0.,0.,1.));
#1745=DIRECTION('',(1.,0.,0.));
#1746=DIRECTION('axis',(0.,0.,1.));
#1747=DIRECTION('refdir',(1.,0.,0.));
#1748=DIRECTION('center_axis',(0.,0.,1.));
#1749=DIRECTION('ref_axis',(1.,0.,0.));
#1750=DIRECTION('center_axis',(0.,0.,-1.));
#1751=DIRECTION('ref_axis',(1.,0.,0.));
#1752=DIRECTION('',(0.,0.,1.));
#1753=DIRECTION('center_axis',(0.,0.,-1.));
#1754=DIRECTION('ref_axis',(1.,0.,0.));
#1755=DIRECTION('center_axis',(0.,0.,1.));
#1756=DIRECTION('ref_axis',(1.,0.,0.));
#1757=DIRECTION('center_axis',(0.,0.,1.));
#1758=DIRECTION('ref_axis',(1.,0.,0.));
#1759=DIRECTION('',(0.,0.,-1.));
#1760=DIRECTION('center_axis',(0.,0.,1.));
#1761=DIRECTION('ref_axis',(1.,0.,0.));
#1762=DIRECTION('center_axis',(0.,0.,1.));
#1763=DIRECTION('ref_axis',(1.,0.,0.));
#1764=DIRECTION('center_axis',(0.,0.,1.));
#1765=DIRECTION('ref_axis',(1.,0.,0.));
#1766=DIRECTION('axis',(0.,0.,1.));
#1767=DIRECTION('refdir',(1.,0.,0.));
#1768=DIRECTION('center_axis',(0.,1.,0.));
#1769=DIRECTION('ref_axis',(1.,0.,0.));
#1770=DIRECTION('center_axis',(0.,-1.,0.));
#1771=DIRECTION('ref_axis',(1.,0.,0.));
#1772=DIRECTION('',(0.,1.,0.));
#1773=DIRECTION('center_axis',(0.,-1.,0.));
#1774=DIRECTION('ref_axis',(1.,0.,0.));
#1775=DIRECTION('center_axis',(0.,1.,0.));
#1776=DIRECTION('ref_axis',(1.,0.,0.));
#1777=DIRECTION('center_axis',(0.,1.,0.));
#1778=DIRECTION('ref_axis',(1.,0.,0.));
#1779=DIRECTION('',(0.,-1.,0.));
#1780=DIRECTION('center_axis',(0.,1.,0.));
#1781=DIRECTION('ref_axis',(1.,0.,0.));
#1782=DIRECTION('center_axis',(0.,1.,0.));
#1783=DIRECTION('ref_axis',(1.,0.,0.));
#1784=DIRECTION('center_axis',(0.,1.,0.));
#1785=DIRECTION('ref_axis',(1.,0.,0.));
#1786=DIRECTION('axis',(0.,0.,1.));
#1787=DIRECTION('refdir',(1.,0.,0.));
#1788=DIRECTION('center_axis',(0.866025403784439,0.,-0.5));
#1789=DIRECTION('ref_axis',(0.5,0.,0.866025403784439));
#1790=DIRECTION('',(-0.5,0.,-0.866025403784439));
#1791=DIRECTION('',(0.,-1.,0.));
#1792=DIRECTION('',(0.5,0.,0.866025403784439));
#1793=DIRECTION('',(0.,-1.,0.));
#1794=DIRECTION('center_axis',(1.60246890531964E-16,0.,-1.));
#1795=DIRECTION('ref_axis',(1.,0.,1.60246890531964E-16));
#1796=DIRECTION('',(-1.,0.,-1.60246890531964E-16));
#1797=DIRECTION('',(0.,-1.,0.));
#1798=DIRECTION('',(1.,0.,1.60246890531964E-16));
#1799=DIRECTION('center_axis',(-0.866025403784439,0.,-0.5));
#1800=DIRECTION('ref_axis',(0.5,0.,-0.866025403784439));
#1801=DIRECTION('',(-0.5,0.,0.866025403784439));
#1802=DIRECTION('',(0.,-1.,0.));
#1803=DIRECTION('',(0.5,0.,-0.866025403784439));
#1804=DIRECTION('center_axis',(-0.866025403784439,0.,0.5));
#1805=DIRECTION('ref_axis',(-0.5,0.,-0.866025403784439));
#1806=DIRECTION('',(0.5,0.,0.866025403784439));
#1807=DIRECTION('',(0.,-1.,0.));
#1808=DIRECTION('',(-0.5,0.,-0.866025403784439));
#1809=DIRECTION('center_axis',(-1.60246890531964E-16,0.,1.));
#1810=DIRECTION('ref_axis',(-1.,0.,-1.60246890531964E-16));
#1811=DIRECTION('',(1.,0.,1.60246890531964E-16));
#1812=DIRECTION('',(0.,-1.,0.));
#1813=DIRECTION('',(-1.,0.,-1.60246890531964E-16));
#1814=DIRECTION('center_axis',(0.866025403784439,0.,0.5));
#1815=DIRECTION('ref_axis',(-0.5,0.,0.866025403784439));
#1816=DIRECTION('',(0.5,0.,-0.866025403784439));
#1817=DIRECTION('',(-0.5,0.,0.866025403784439));
#1818=DIRECTION('center_axis',(0.,1.,0.));
#1819=DIRECTION('ref_axis',(1.,0.,0.));
#1820=DIRECTION('center_axis',(0.,-1.,0.));
#1821=DIRECTION('ref_axis',(0.,0.,-1.));
#1822=DIRECTION('center_axis',(0.,1.,0.));
#1823=DIRECTION('ref_axis',(0.,0.,1.));
#1824=DIRECTION('center_axis',(0.,-1.,0.));
#1825=DIRECTION('ref_axis',(1.,0.,0.));
#1826=DIRECTION('center_axis',(0.,-1.,0.));
#1827=DIRECTION('ref_axis',(1.,0.,0.));
#1828=DIRECTION('center_axis',(0.,-1.,0.));
#1829=DIRECTION('ref_axis',(1.,0.,0.));
#1830=DIRECTION('',(0.707106781186547,0.707106781186548,8.65956056235493E-17));
#1831=DIRECTION('center_axis',(0.,-1.,0.));
#1832=DIRECTION('ref_axis',(1.,0.,0.));
#1833=DIRECTION('center_axis',(0.,-1.,0.));
#1834=DIRECTION('ref_axis',(1.,0.,0.));
#1835=DIRECTION('',(0.,1.,0.));
#1836=DIRECTION('center_axis',(0.,1.,0.));
#1837=DIRECTION('ref_axis',(1.,0.,0.));
#1838=DIRECTION('',(0.707106781186548,-0.707106781186547,-8.65956056235494E-17));
#1839=DIRECTION('center_axis',(0.,-1.,0.));
#1840=DIRECTION('ref_axis',(1.,0.,0.));
#1841=DIRECTION('center_axis',(0.,-1.,0.));
#1842=DIRECTION('ref_axis',(0.,0.,-1.));
#1843=DIRECTION('center_axis',(0.,-1.,0.));
#1844=DIRECTION('ref_axis',(1.,0.,0.));
#1845=DIRECTION('center_axis',(0.,1.,0.));
#1846=DIRECTION('ref_axis',(1.,0.,0.));
#1847=DIRECTION('',(0.447213595499958,-0.894427190999916,-5.47678698264203E-17));
#1848=DIRECTION('center_axis',(0.,1.,0.));
#1849=DIRECTION('ref_axis',(1.,0.,0.));
#1850=DIRECTION('center_axis',(0.,-1.,0.));
#1851=DIRECTION('ref_axis',(1.,0.,0.));
#1852=DIRECTION('center_axis',(0.,1.,0.));
#1853=DIRECTION('ref_axis',(1.,0.,0.));
#1854=DIRECTION('',(0.,1.,0.));
#1855=DIRECTION('center_axis',(0.,1.,0.));
#1856=DIRECTION('ref_axis',(1.,0.,0.));
#1857=DIRECTION('',(0.707106781186547,-0.707106781186548,-8.65956056235493E-17));
#1858=DIRECTION('center_axis',(0.,-1.,0.));
#1859=DIRECTION('ref_axis',(1.,0.,0.));
#1860=DIRECTION('center_axis',(0.,-1.,0.));
#1861=DIRECTION('ref_axis',(0.,0.,-1.));
#1862=DIRECTION('axis',(0.,0.,1.));
#1863=DIRECTION('refdir',(1.,0.,0.));
#1864=DIRECTION('center_axis',(0.,1.,0.));
#1865=DIRECTION('ref_axis',(1.,0.,0.));
#1866=DIRECTION('center_axis',(0.,-1.,0.));
#1867=DIRECTION('ref_axis',(1.,0.,0.));
#1868=DIRECTION('center_axis',(0.,1.,0.));
#1869=DIRECTION('ref_axis',(1.,0.,0.));
#1870=DIRECTION('center_axis',(0.,1.,0.));
#1871=DIRECTION('ref_axis',(1.,0.,0.));
#1872=DIRECTION('',(0.,-1.,0.));
#1873=DIRECTION('center_axis',(0.,1.,0.));
#1874=DIRECTION('ref_axis',(1.,0.,0.));
#1875=DIRECTION('',(0.,0.,1.));
#1876=DIRECTION('',(1.,0.,0.));
#1877=DIRECTION('',(0.,0.,1.));
#1878=DIRECTION('',(1.,0.,0.));
#1879=DIRECTION('',(0.,0.,1.));
#1880=DIRECTION('',(1.,0.,0.));
#1881=DIRECTION('',(0.,-1.,2.22044604925031E-16));
#1882=DIRECTION('',(1.,0.,0.));
#1883=DIRECTION('',(0.,-1.,2.22044604925031E-16));
#1884=DIRECTION('',(1.,0.,0.));
#1885=DIRECTION('',(0.,0.,1.));
#1886=DIRECTION('',(1.,0.,0.));
#1887=DIRECTION('',(0.,-1.,2.22044604925031E-16));
#1888=DIRECTION('',(1.,0.,0.));
#1889=DIRECTION('',(0.,-1.,2.22044604925031E-16));
#1890=DIRECTION('',(1.,0.,0.));
#1891=DIRECTION('',(0.,0.,1.));
#1892=DIRECTION('',(1.,0.,0.));
#1893=DIRECTION('',(0.,0.,1.));
#1894=DIRECTION('',(1.,0.,0.));
#1895=DIRECTION('',(0.,-1.,2.22044604925031E-16));
#1896=DIRECTION('',(1.,0.,0.));
#1897=DIRECTION('',(0.,-1.,2.22044604925031E-16));
#1898=DIRECTION('',(1.,0.,0.));
#1899=DIRECTION('',(0.,0.,1.));
#1900=DIRECTION('',(1.,0.,0.));
#1901=DIRECTION('',(0.,-1.,2.22044604925031E-16));
#1902=DIRECTION('',(1.,0.,0.));
#1903=DIRECTION('',(0.,-1.,2.22044604925031E-16));
#1904=DIRECTION('',(1.,0.,0.));
#1905=DIRECTION('',(0.,0.,1.));
#1906=DIRECTION('',(1.,0.,0.));
#1907=CARTESIAN_POINT('',(0.,0.,0.));
#1908=CARTESIAN_POINT('',(0.,0.,0.));
#1909=CARTESIAN_POINT('Origin',(4.75,20.,-0.5));
#1910=CARTESIAN_POINT('',(4.41,20.,-0.5));
#1911=CARTESIAN_POINT('Origin',(4.75,20.,-0.5));
#1912=CARTESIAN_POINT('',(4.41,20.,1.2));
#1913=CARTESIAN_POINT('',(4.41,20.,-0.5));
#1914=CARTESIAN_POINT('Origin',(4.75,20.,1.2));
#1915=CARTESIAN_POINT('Origin',(4.75,20.,-0.5));
#1916=CARTESIAN_POINT('Origin',(-4.75,20.,-0.5));
#1917=CARTESIAN_POINT('',(-5.09,20.,-0.5));
#1918=CARTESIAN_POINT('Origin',(-4.75,20.,-0.5));
#1919=CARTESIAN_POINT('',(-5.09,20.,1.2));
#1920=CARTESIAN_POINT('',(-5.09,20.,-0.5));
#1921=CARTESIAN_POINT('Origin',(-4.75,20.,1.2));
#1922=CARTESIAN_POINT('Origin',(-4.75,20.,-0.5));
#1923=CARTESIAN_POINT('Origin',(4.75,0.,-0.5));
#1924=CARTESIAN_POINT('',(4.41,-4.163799117101E-17,-0.5));
#1925=CARTESIAN_POINT('Origin',(4.75,0.,-0.5));
#1926=CARTESIAN_POINT('',(4.41,4.163799117101E-17,1.2));
#1927=CARTESIAN_POINT('',(4.41,-4.163799117101E-17,-0.5));
#1928=CARTESIAN_POINT('Origin',(4.75,0.,1.2));
#1929=CARTESIAN_POINT('Origin',(4.75,0.,-0.5));
#1930=CARTESIAN_POINT('Origin',(-4.75,0.,-0.5));
#1931=CARTESIAN_POINT('',(-5.09,-4.163799117101E-17,-0.5));
#1932=CARTESIAN_POINT('Origin',(-4.75,0.,-0.5));
#1933=CARTESIAN_POINT('',(-5.09,4.163799117101E-17,1.2));
#1934=CARTESIAN_POINT('',(-5.09,-4.163799117101E-17,-0.5));
#1935=CARTESIAN_POINT('Origin',(-4.75,0.,1.2));
#1936=CARTESIAN_POINT('Origin',(-4.75,0.,-0.5));
#1937=CARTESIAN_POINT('Origin',(8.,24.5,-0.6));
#1938=CARTESIAN_POINT('',(8.,24.5,-0.6));
#1939=CARTESIAN_POINT('',(-8.,24.5,-0.6));
#1940=CARTESIAN_POINT('',(8.,24.5,-0.6));
#1941=CARTESIAN_POINT('',(-8.,24.5,1.2));
#1942=CARTESIAN_POINT('',(-8.,24.5,-0.6));
#1943=CARTESIAN_POINT('',(8.,24.5,1.2));
#1944=CARTESIAN_POINT('',(8.,24.5,1.2));
#1945=CARTESIAN_POINT('',(8.,24.5,-0.6));
#1946=CARTESIAN_POINT('Origin',(8.,-4.5,-0.6));
#1947=CARTESIAN_POINT('',(8.,-4.5,-0.6));
#1948=CARTESIAN_POINT('',(8.,-4.5,-0.6));
#1949=CARTESIAN_POINT('',(8.,-4.5,1.2));
#1950=CARTESIAN_POINT('',(8.,-4.5,1.2));
#1951=CARTESIAN_POINT('',(8.,-4.5,-0.6));
#1952=CARTESIAN_POINT('Origin',(-8.,-4.5,-0.6));
#1953=CARTESIAN_POINT('',(-8.,-4.5,-0.6));
#1954=CARTESIAN_POINT('',(-8.,-4.5,-0.6));
#1955=CARTESIAN_POINT('',(-8.,-4.5,1.2));
#1956=CARTESIAN_POINT('',(-8.,-4.5,1.2));
#1957=CARTESIAN_POINT('',(-8.,-4.5,-0.6));
#1958=CARTESIAN_POINT('Origin',(-8.,24.5,-0.6));
#1959=CARTESIAN_POINT('',(-8.,24.5,-0.6));
#1960=CARTESIAN_POINT('',(-8.,24.5,1.2));
#1961=CARTESIAN_POINT('Origin',(0.,10.,1.2));
#1962=CARTESIAN_POINT('Origin',(0.,10.,-0.6));
#1963=CARTESIAN_POINT('',(0.,0.,0.));
#1964=CARTESIAN_POINT('',(0.,0.,0.));
#1965=CARTESIAN_POINT('Origin',(0.,0.,0.));
#1966=CARTESIAN_POINT('',(-2.05,-1.65,2.51052593825207E-16));
#1967=CARTESIAN_POINT('Origin',(0.,-1.65,0.));
#1968=CARTESIAN_POINT('',(-2.05,-1.14891252930761,-2.51052593825207E-16));
#1969=CARTESIAN_POINT('',(-2.05,0.,2.51052593825207E-16));
#1970=CARTESIAN_POINT('Origin',(0.,-1.14891252930761,0.));
#1971=CARTESIAN_POINT('Origin',(0.,0.,0.));
#1972=CARTESIAN_POINT('',(-2.05,1.14891252930761,2.51052593825207E-16));
#1973=CARTESIAN_POINT('Origin',(0.,1.14891252930761,0.));
#1974=CARTESIAN_POINT('',(-2.05,1.65,-2.51052593825207E-16));
#1975=CARTESIAN_POINT('',(-2.05,0.,2.51052593825207E-16));
#1976=CARTESIAN_POINT('Origin',(0.,1.65,0.));
#1977=CARTESIAN_POINT('Origin',(0.,0.,0.));
#1978=CARTESIAN_POINT('',(-2.87791997799628E-16,-1.76221774462768E-32,-2.35));
#1979=CARTESIAN_POINT('',(7.39557098644699E-32,-1.76221774462768E-32,2.35));
#1980=CARTESIAN_POINT('Origin',(0.,0.,0.));
#1981=CARTESIAN_POINT('Origin',(0.,1.55,-1.49));
#1982=CARTESIAN_POINT('',(-3.76384615384615,1.55,-2.13));
#1983=CARTESIAN_POINT('',(-1.81744325908679,1.55,-2.13));
#1984=CARTESIAN_POINT('',(0.,1.55,-2.13));
#1985=CARTESIAN_POINT('',(-2.46585583768694,1.55,-1.32648218523477));
#1986=CARTESIAN_POINT('',(-1.68,1.55,-0.84));
#1987=CARTESIAN_POINT('Origin',(0.,1.55,0.));
#1988=CARTESIAN_POINT('Origin',(0.,1.55,-1.49));
#1989=CARTESIAN_POINT('',(1.81744325908679,1.55,-2.13));
#1990=CARTESIAN_POINT('',(3.76384615384615,1.55,-2.13));
#1991=CARTESIAN_POINT('',(0.,1.55,-2.13));
#1992=CARTESIAN_POINT('',(2.46585583768694,1.55,-1.32648218523477));
#1993=CARTESIAN_POINT('Origin',(0.,1.55,0.));
#1994=CARTESIAN_POINT('',(3.78,1.55,-2.14));
#1995=CARTESIAN_POINT('Origin',(0.,-1.55,-1.49));
#1996=CARTESIAN_POINT('',(-1.81744325908679,-1.55,-2.13));
#1997=CARTESIAN_POINT('',(-3.76384615384615,-1.55,-2.13));
#1998=CARTESIAN_POINT('',(0.,-1.55,-2.13));
#1999=CARTESIAN_POINT('',(-2.46585583768694,-1.55,-1.32648218523477));
#2000=CARTESIAN_POINT('Origin',(0.,-1.55,0.));
#2001=CARTESIAN_POINT('',(-1.68,-1.55,-0.84));
#2002=CARTESIAN_POINT('Origin',(-3.78,0.,-2.14));
#2003=CARTESIAN_POINT('',(-3.76384615384615,0.,-2.13));
#2004=CARTESIAN_POINT('',(-2.46585583768694,0.,-1.32648218523477));
#2005=CARTESIAN_POINT('Origin',(0.,-1.55,-1.49));
#2006=CARTESIAN_POINT('',(3.76384615384615,-1.55,-2.13));
#2007=CARTESIAN_POINT('',(1.81744325908679,-1.55,-2.13));
#2008=CARTESIAN_POINT('',(0.,-1.55,-2.13));
#2009=CARTESIAN_POINT('',(2.46585583768694,-1.55,-1.32648218523477));
#2010=CARTESIAN_POINT('',(3.78,-1.55,-2.14));
#2011=CARTESIAN_POINT('Origin',(0.,-1.55,0.));
#2012=CARTESIAN_POINT('Origin',(1.68,0.,-0.84));
#2013=CARTESIAN_POINT('',(3.76384615384615,0.,-2.13));
#2014=CARTESIAN_POINT('',(2.46585583768694,0.,-1.32648218523477));
#2015=CARTESIAN_POINT('Origin',(0.,0.,-2.13));
#2016=CARTESIAN_POINT('',(-6.35,1.9,-2.13));
#2017=CARTESIAN_POINT('',(-6.35,-1.9,-2.13));
#2018=CARTESIAN_POINT('',(-6.35,1.9,-2.13));
#2019=CARTESIAN_POINT('',(6.35,-1.9,-2.13));
#2020=CARTESIAN_POINT('',(-6.35,-1.9,-2.13));
#2021=CARTESIAN_POINT('',(6.35,1.9,-2.13));
#2022=CARTESIAN_POINT('',(6.35,-1.9,-2.13));
#2023=CARTESIAN_POINT('',(6.35,1.9,-2.13));
#2024=CARTESIAN_POINT('',(4.1,7.9602041944578E-17,-2.13));
#2025=CARTESIAN_POINT('Origin',(4.75,0.,-2.13));
#2026=CARTESIAN_POINT('',(-5.4,7.9602041944578E-17,-2.13));
#2027=CARTESIAN_POINT('Origin',(-4.75,0.,-2.13));
#2028=CARTESIAN_POINT('',(1.81744325908679,-1.65,-2.13));
#2029=CARTESIAN_POINT('',(1.81744325908679,0.,-2.13));
#2030=CARTESIAN_POINT('',(-1.81744325908679,-1.65,-2.13));
#2031=CARTESIAN_POINT('',(0.,-1.65,-2.13));
#2032=CARTESIAN_POINT('',(-1.81744325908679,0.,-2.13));
#2033=CARTESIAN_POINT('',(-1.81744325908679,1.65,-2.13));
#2034=CARTESIAN_POINT('',(-1.81744325908679,0.,-2.13));
#2035=CARTESIAN_POINT('',(1.81744325908679,1.65,-2.13));
#2036=CARTESIAN_POINT('',(0.,1.65,-2.13));
#2037=CARTESIAN_POINT('',(1.81744325908679,0.,-2.13));
#2038=CARTESIAN_POINT('Origin',(0.,0.,0.));
#2039=CARTESIAN_POINT('Origin',(0.,1.65,0.));
#2040=CARTESIAN_POINT('Origin',(0.,-1.65,0.));
#2041=CARTESIAN_POINT('Origin',(0.,-1.65,0.));
#2042=CARTESIAN_POINT('Origin',(0.,1.65,0.));
#2043=CARTESIAN_POINT('Origin',(3.35,1.4,-3.33));
#2044=CARTESIAN_POINT('',(3.35,1.4,-3.33));
#2045=CARTESIAN_POINT('',(-3.35,1.4,-3.33));
#2046=CARTESIAN_POINT('',(1.675,1.4,-3.33));
#2047=CARTESIAN_POINT('',(3.35,1.4,-2.83));
#2048=CARTESIAN_POINT('',(3.35,1.4,-3.33));
#2049=CARTESIAN_POINT('',(-3.35,1.4,-2.83));
#2050=CARTESIAN_POINT('',(3.35,1.4,-2.83));
#2051=CARTESIAN_POINT('',(-3.35,1.4,-3.33));
#2052=CARTESIAN_POINT('Origin',(3.35,-1.4,-3.33));
#2053=CARTESIAN_POINT('',(3.35,-1.4,-3.33));
#2054=CARTESIAN_POINT('',(3.35,-0.7,-3.33));
#2055=CARTESIAN_POINT('',(3.35,-1.4,-2.83));
#2056=CARTESIAN_POINT('',(3.35,-1.4,-3.33));
#2057=CARTESIAN_POINT('',(3.35,-1.4,-2.83));
#2058=CARTESIAN_POINT('Origin',(-3.35,-1.4,-3.33));
#2059=CARTESIAN_POINT('',(-3.35,-1.4,-3.33));
#2060=CARTESIAN_POINT('',(-1.675,-1.4,-3.33));
#2061=CARTESIAN_POINT('',(-3.35,-1.4,-2.83));
#2062=CARTESIAN_POINT('',(-3.35,-1.4,-3.33));
#2063=CARTESIAN_POINT('',(-3.35,-1.4,-2.83));
#2064=CARTESIAN_POINT('Origin',(-3.35,1.4,-3.33));
#2065=CARTESIAN_POINT('',(-3.35,0.7,-3.33));
#2066=CARTESIAN_POINT('',(-3.35,1.4,-2.83));
#2067=CARTESIAN_POINT('Origin',(0.,0.,-2.83));
#2068=CARTESIAN_POINT('Origin',(-4.75,0.,-3.33));
#2069=CARTESIAN_POINT('',(-5.4,-7.9602041944578E-17,-3.33));
#2070=CARTESIAN_POINT('Origin',(-4.75,0.,-3.33));
#2071=CARTESIAN_POINT('',(-5.4,-7.9602041944578E-17,-3.33));
#2072=CARTESIAN_POINT('Origin',(4.75,0.,-3.33));
#2073=CARTESIAN_POINT('',(4.1,-7.9602041944578E-17,-3.33));
#2074=CARTESIAN_POINT('Origin',(4.75,0.,-3.33));
#2075=CARTESIAN_POINT('',(4.1,-7.9602041944578E-17,-3.33));
#2076=CARTESIAN_POINT('Origin',(6.35,1.9,-3.33));
#2077=CARTESIAN_POINT('',(6.35,1.9,-3.33));
#2078=CARTESIAN_POINT('',(-6.35,1.9,-3.33));
#2079=CARTESIAN_POINT('',(6.35,1.9,-3.33));
#2080=CARTESIAN_POINT('',(-6.35,1.9,-3.33));
#2081=CARTESIAN_POINT('',(6.35,1.9,-3.33));
#2082=CARTESIAN_POINT('Origin',(6.35,-1.9,-3.33));
#2083=CARTESIAN_POINT('',(6.35,-1.9,-3.33));
#2084=CARTESIAN_POINT('',(6.35,-1.9,-3.33));
#2085=CARTESIAN_POINT('',(6.35,-1.9,-3.33));
#2086=CARTESIAN_POINT('Origin',(-6.35,-1.9,-3.33));
#2087=CARTESIAN_POINT('',(-6.35,-1.9,-3.33));
#2088=CARTESIAN_POINT('',(-6.35,-1.9,-3.33));
#2089=CARTESIAN_POINT('',(-6.35,-1.9,-3.33));
#2090=CARTESIAN_POINT('Origin',(-6.35,1.9,-3.33));
#2091=CARTESIAN_POINT('',(-6.35,1.9,-3.33));
#2092=CARTESIAN_POINT('Origin',(0.,0.,-3.33));
#2093=CARTESIAN_POINT('',(0.,0.,0.));
#2094=CARTESIAN_POINT('Origin',(0.,0.,0.));
#2095=CARTESIAN_POINT('',(-1.8,0.85,-2.20436423846524E-16));
#2096=CARTESIAN_POINT('Origin',(0.,0.85,0.));
#2097=CARTESIAN_POINT('',(-1.8,-0.85,-2.20436423846524E-16));
#2098=CARTESIAN_POINT('',(-1.8,0.,-2.20436423846524E-16));
#2099=CARTESIAN_POINT('Origin',(0.,-0.85,0.));
#2100=CARTESIAN_POINT('Origin',(2.19089023002066,0.85,0.));
#2101=CARTESIAN_POINT('',(2.19089023002066,0.85,0.));
#2102=CARTESIAN_POINT('Origin',(0.,0.85,0.));
#2103=CARTESIAN_POINT('Origin',(3.99680288865056E-15,0.,0.));
#2104=CARTESIAN_POINT('',(3.99680288865056E-15,-1.76221774462768E-32,2.35));
#2105=CARTESIAN_POINT('',(3.70901089085093E-15,-1.76221774462768E-32,-2.35));
#2106=CARTESIAN_POINT('Origin',(3.99680288865056E-15,0.,0.));
#2107=CARTESIAN_POINT('',(2.19089023002066,-0.85,0.));
#2108=CARTESIAN_POINT('Origin',(0.,-0.85,0.));
#2109=CARTESIAN_POINT('Origin',(1.8,-0.85,0.));
#2110=CARTESIAN_POINT('Origin',(0.,1.55,0.));
#2111=CARTESIAN_POINT('',(-1.65,0.85,-2.02066721859313E-16));
#2112=CARTESIAN_POINT('Origin',(0.,0.85,0.));
#2113=CARTESIAN_POINT('',(-1.65,2.25,-2.02066721859313E-16));
#2114=CARTESIAN_POINT('',(-1.65,1.55,-2.02066721859313E-16));
#2115=CARTESIAN_POINT('Origin',(0.,2.25,0.));
#2116=CARTESIAN_POINT('Origin',(1.65,2.25,0.));
#2117=CARTESIAN_POINT('',(-1.,2.25,-1.22464679914735E-16));
#2118=CARTESIAN_POINT('Origin',(0.,2.25,0.));
#2119=CARTESIAN_POINT('Origin',(1.75,0.85,0.));
#2120=CARTESIAN_POINT('',(-1.75,0.85,-2.14313189850787E-16));
#2121=CARTESIAN_POINT('Origin',(0.,0.85,0.));
#2122=CARTESIAN_POINT('Origin',(0.,0.,0.));
#2123=CARTESIAN_POINT('',(-1.75,-0.85,-2.14313189850787E-16));
#2124=CARTESIAN_POINT('Origin',(0.,-0.85,0.));
#2125=CARTESIAN_POINT('',(-1.75,0.,-2.14313189850787E-16));
#2126=CARTESIAN_POINT('Origin',(1.,-0.85,0.));
#2127=CARTESIAN_POINT('',(-1.,-0.85,-1.22464679914735E-16));
#2128=CARTESIAN_POINT('Origin',(0.,-0.85,0.));
#2129=CARTESIAN_POINT('Origin',(0.,0.7,0.));
#2130=CARTESIAN_POINT('',(-1.,0.7,-1.22464679914735E-16));
#2131=CARTESIAN_POINT('',(0.,0.,0.));
#2132=CARTESIAN_POINT('',(0.,0.,0.));
#2133=CARTESIAN_POINT('',(0.,0.,0.));
#2134=CARTESIAN_POINT('Origin',(-4.75,0.,1.2));
#2135=CARTESIAN_POINT('',(-5.175,-5.20474889637625E-17,1.2));
#2136=CARTESIAN_POINT('Origin',(-4.75,0.,1.2));
#2137=CARTESIAN_POINT('',(-5.175,-5.20474889637625E-17,2.4));
#2138=CARTESIAN_POINT('',(-5.175,-5.20474889637625E-17,1.2));
#2139=CARTESIAN_POINT('Origin',(-4.75,0.,2.4));
#2140=CARTESIAN_POINT('Origin',(-4.75,0.,1.2));
#2141=CARTESIAN_POINT('',(-5.395,-7.89897185450042E-17,2.4));
#2142=CARTESIAN_POINT('Origin',(-4.75,0.,2.4));
#2143=CARTESIAN_POINT('',(-5.395,-7.89897185450042E-17,1.2));
#2144=CARTESIAN_POINT('',(-5.395,-7.89897185450043E-17,1.2));
#2145=CARTESIAN_POINT('Origin',(-4.75,0.,1.2));
#2146=CARTESIAN_POINT('Origin',(-4.75,0.,2.4));
#2147=CARTESIAN_POINT('Origin',(-4.75,0.,1.2));
#2148=CARTESIAN_POINT('',(0.,0.,0.));
#2149=CARTESIAN_POINT('Origin',(0.,0.,0.));
#2150=CARTESIAN_POINT('',(-0.42,0.,5.14351655641888E-17));
#2151=CARTESIAN_POINT('Origin',(0.,0.,0.));
#2152=CARTESIAN_POINT('',(-0.42,0.16,5.14351655641888E-17));
#2153=CARTESIAN_POINT('',(-0.42,0.,5.14351655641888E-17));
#2154=CARTESIAN_POINT('Origin',(0.,0.16,0.));
#2155=CARTESIAN_POINT('Origin',(0.,0.,0.));
#2156=CARTESIAN_POINT('',(-0.8,0.16,9.79717439317883E-17));
#2157=CARTESIAN_POINT('Origin',(0.,0.16,0.));
#2158=CARTESIAN_POINT('',(-0.8,0.,9.79717439317883E-17));
#2159=CARTESIAN_POINT('',(-0.8,0.,9.79717439317883E-17));
#2160=CARTESIAN_POINT('Origin',(0.,0.,0.));
#2161=CARTESIAN_POINT('Origin',(0.,0.16,0.));
#2162=CARTESIAN_POINT('Origin',(0.,0.,0.));
#2163=CARTESIAN_POINT('',(0.,0.,0.));
#2164=CARTESIAN_POINT('Origin',(0.173205080756888,-0.8,-0.3));
#2165=CARTESIAN_POINT('',(0.346410161513775,-0.8,0.));
#2166=CARTESIAN_POINT('',(0.173205080756888,-0.8,-0.3));
#2167=CARTESIAN_POINT('',(0.346410161513775,-0.8,0.));
#2168=CARTESIAN_POINT('',(0.173205080756888,-1.28,-0.3));
#2169=CARTESIAN_POINT('',(0.173205080756888,-0.8,-0.3));
#2170=CARTESIAN_POINT('',(0.346410161513775,-1.28,0.));
#2171=CARTESIAN_POINT('',(0.346410161513775,-1.28,0.));
#2172=CARTESIAN_POINT('',(0.346410161513775,-0.8,0.));
#2173=CARTESIAN_POINT('Origin',(-0.173205080756888,-0.8,-0.3));
#2174=CARTESIAN_POINT('',(-0.173205080756888,-0.8,-0.3));
#2175=CARTESIAN_POINT('',(0.173205080756888,-0.8,-0.3));
#2176=CARTESIAN_POINT('',(-0.173205080756888,-1.28,-0.3));
#2177=CARTESIAN_POINT('',(-0.173205080756888,-0.8,-0.3));
#2178=CARTESIAN_POINT('',(0.173205080756888,-1.28,-0.3));
#2179=CARTESIAN_POINT('Origin',(-0.346410161513775,-0.8,-5.55111512312578E-17));
#2180=CARTESIAN_POINT('',(-0.346410161513775,-0.8,-4.24230095489963E-17));
#2181=CARTESIAN_POINT('',(-0.173205080756888,-0.8,-0.3));
#2182=CARTESIAN_POINT('',(-0.346410161513775,-1.28,-5.55111512312578E-17));
#2183=CARTESIAN_POINT('',(-0.346410161513775,-0.8,-4.24230095489963E-17));
#2184=CARTESIAN_POINT('',(-0.173205080756888,-1.28,-0.3));
#2185=CARTESIAN_POINT('Origin',(-0.173205080756888,-0.8,0.3));
#2186=CARTESIAN_POINT('',(-0.173205080756888,-0.8,0.3));
#2187=CARTESIAN_POINT('',(-0.346410161513775,-0.8,-4.24230095489963E-17));
#2188=CARTESIAN_POINT('',(-0.173205080756888,-1.28,0.3));
#2189=CARTESIAN_POINT('',(-0.173205080756888,-0.8,0.3));
#2190=CARTESIAN_POINT('',(-0.346410161513775,-1.28,-4.24230095489963E-17));
#2191=CARTESIAN_POINT('Origin',(0.173205080756888,-0.8,0.3));
#2192=CARTESIAN_POINT('',(0.173205080756888,-0.8,0.3));
#2193=CARTESIAN_POINT('',(-0.173205080756888,-0.8,0.3));
#2194=CARTESIAN_POINT('',(0.173205080756888,-1.28,0.3));
#2195=CARTESIAN_POINT('',(0.173205080756888,-0.8,0.3));
#2196=CARTESIAN_POINT('',(-0.173205080756888,-1.28,0.3));
#2197=CARTESIAN_POINT('Origin',(0.346410161513775,-0.8,0.));
#2198=CARTESIAN_POINT('',(0.173205080756888,-0.8,0.3));
#2199=CARTESIAN_POINT('',(0.173205080756888,-1.28,0.3));
#2200=CARTESIAN_POINT('Origin',(0.,-0.8,-5.55111512312578E-17));
#2201=CARTESIAN_POINT('Origin',(0.,-1.28,-5.55111512312578E-17));
#2202=CARTESIAN_POINT('Origin',(0.6,0.8,0.));
#2203=CARTESIAN_POINT('',(-0.6,0.8,-7.34788079488412E-17));
#2204=CARTESIAN_POINT('Origin',(0.,0.8,0.));
#2205=CARTESIAN_POINT('Origin',(0.,0.775,0.));
#2206=CARTESIAN_POINT('',(-0.65,0.75,-7.9602041944578E-17));
#2207=CARTESIAN_POINT('Origin',(0.,0.75,0.));
#2208=CARTESIAN_POINT('',(-0.625,0.775,-7.65404249467096E-17));
#2209=CARTESIAN_POINT('Origin',(0.,0.39,0.));
#2210=CARTESIAN_POINT('',(-0.65,0.0299999999999998,-7.9602041944578E-17));
#2211=CARTESIAN_POINT('Origin',(0.,0.0299999999999998,0.));
#2212=CARTESIAN_POINT('',(-0.65,0.39,-7.9602041944578E-17));
#2213=CARTESIAN_POINT('Origin',(0.,0.0150000000000001,0.));
#2214=CARTESIAN_POINT('',(-0.62,5.89805981832114E-17,-7.59281015471359E-17));
#2215=CARTESIAN_POINT('',(-0.635,0.0150000000000001,7.77650717458569E-17));
#2216=CARTESIAN_POINT('Origin',(0.,0.,0.));
#2217=CARTESIAN_POINT('Origin',(0.42,0.,0.));
#2218=CARTESIAN_POINT('',(-0.42,-3.46944695195361E-18,-5.14351655641888E-17));
#2219=CARTESIAN_POINT('Origin',(0.,0.,0.));
#2220=CARTESIAN_POINT('Origin',(0.,-0.02,0.));
#2221=CARTESIAN_POINT('',(-0.3933,-0.0534000000000001,4.81653586104654E-17));
#2222=CARTESIAN_POINT('',(-0.41,-0.02,5.02105187650415E-17));
#2223=CARTESIAN_POINT('Origin',(0.,-0.0534000000000001,0.));
#2224=CARTESIAN_POINT('Origin',(0.,-1.48,0.));
#2225=CARTESIAN_POINT('',(-0.3933,-2.9267,4.81653586104654E-17));
#2226=CARTESIAN_POINT('Origin',(0.,-2.9267,0.));
#2227=CARTESIAN_POINT('',(-0.3933,-1.48,-4.81653586104654E-17));
#2228=CARTESIAN_POINT('Origin',(0.,-2.96,0.));
#2229=CARTESIAN_POINT('',(-0.32,-3.,-3.91886975727153E-17));
#2230=CARTESIAN_POINT('',(-0.36,-2.96,4.40872847693047E-17));
#2231=CARTESIAN_POINT('Origin',(0.,-3.,0.));
#2232=CARTESIAN_POINT('Origin',(0.,-3.,0.));
#2233=CARTESIAN_POINT('',(0.,0.,0.));
#2234=CARTESIAN_POINT('Origin',(0.,-5.,4.53));
#2235=CARTESIAN_POINT('',(-1.,-5.,4.53));
#2236=CARTESIAN_POINT('Origin',(0.,-5.,4.53));
#2237=CARTESIAN_POINT('Origin',(0.,0.,4.53));
#2238=CARTESIAN_POINT('',(-1.,25.,4.53));
#2239=CARTESIAN_POINT('Origin',(0.,25.,4.53));
#2240=CARTESIAN_POINT('',(-1.,0.,4.53));
#2241=CARTESIAN_POINT('Origin',(0.,25.,4.53));
#2242=CARTESIAN_POINT('',(0.,0.,0.));
#2243=CARTESIAN_POINT('',(0.,0.,4.53));
#2244=CARTESIAN_POINT('',(0.,0.,0.));
#2245=CARTESIAN_POINT('',(-4.75,0.,2.4));
#2246=CARTESIAN_POINT('',(-4.75,0.,2.56));
#2247=CARTESIAN_POINT('',(9.5,0.,0.));
#2248=CARTESIAN_POINT('',(4.75,0.,2.4));
#2249=CARTESIAN_POINT('',(4.75,0.,2.56));
#2250=CARTESIAN_POINT('',(0.,20.,4.53));
#2251=CARTESIAN_POINT('',(0.,20.,0.));
#2252=CARTESIAN_POINT('',(-4.75,20.,2.4));
#2253=CARTESIAN_POINT('',(-4.75,20.,2.56));
#2254=CARTESIAN_POINT('',(9.5,20.,0.));
#2255=CARTESIAN_POINT('',(4.75,20.,2.4));
#2256=CARTESIAN_POINT('',(4.75,20.,2.56));
#2257=CARTESIAN_POINT('',(0.,0.,0.));
#2258=UNCERTAINTY_MEASURE_WITH_UNIT(LENGTH_MEASURE(0.001),#2278,
'DISTANCE_ACCURACY_VALUE',
'Maximum model space distance between geometric entities at asserted c
onnectivities');
#2259=UNCERTAINTY_MEASURE_WITH_UNIT(LENGTH_MEASURE(0.001),#2278,
'DISTANCE_ACCURACY_VALUE',
'Maximum model space distance between geometric entities at asserted c
onnectivities');
#2260=UNCERTAINTY_MEASURE_WITH_UNIT(LENGTH_MEASURE(0.001),#2278,
'DISTANCE_ACCURACY_VALUE',
'Maximum model space distance between geometric entities at asserted c
onnectivities');
#2261=UNCERTAINTY_MEASURE_WITH_UNIT(LENGTH_MEASURE(0.001),#2278,
'DISTANCE_ACCURACY_VALUE',
'Maximum model space distance between geometric entities at asserted c
onnectivities');
#2262=UNCERTAINTY_MEASURE_WITH_UNIT(LENGTH_MEASURE(0.001),#2278,
'DISTANCE_ACCURACY_VALUE',
'Maximum model space distance between geometric entities at asserted c
onnectivities');
#2263=UNCERTAINTY_MEASURE_WITH_UNIT(LENGTH_MEASURE(0.001),#2278,
'DISTANCE_ACCURACY_VALUE',
'Maximum model space distance between geometric entities at asserted c
onnectivities');
#2264=UNCERTAINTY_MEASURE_WITH_UNIT(LENGTH_MEASURE(0.001),#2278,
'DISTANCE_ACCURACY_VALUE',
'Maximum model space distance between geometric entities at asserted c
onnectivities');
#2265=UNCERTAINTY_MEASURE_WITH_UNIT(LENGTH_MEASURE(0.001),#2278,
'DISTANCE_ACCURACY_VALUE',
'Maximum model space distance between geometric entities at asserted c
onnectivities');
#2266=UNCERTAINTY_MEASURE_WITH_UNIT(LENGTH_MEASURE(0.001),#2278,
'DISTANCE_ACCURACY_VALUE',
'Maximum model space distance between geometric entities at asserted c
onnectivities');
#2267=UNCERTAINTY_MEASURE_WITH_UNIT(LENGTH_MEASURE(0.001),#2278,
'DISTANCE_ACCURACY_VALUE',
'Maximum model space distance between geometric entities at asserted c
onnectivities');
#2268=(
GEOMETRIC_REPRESENTATION_CONTEXT(3)
GLOBAL_UNCERTAINTY_ASSIGNED_CONTEXT((#2258))
GLOBAL_UNIT_ASSIGNED_CONTEXT((#2278,#2280,#2281))
REPRESENTATION_CONTEXT('','3D')
);
#2269=(
GEOMETRIC_REPRESENTATION_CONTEXT(3)
GLOBAL_UNCERTAINTY_ASSIGNED_CONTEXT((#2259))
GLOBAL_UNIT_ASSIGNED_CONTEXT((#2278,#2280,#2281))
REPRESENTATION_CONTEXT('','3D')
);
#2270=(
GEOMETRIC_REPRESENTATION_CONTEXT(3)
GLOBAL_UNCERTAINTY_ASSIGNED_CONTEXT((#2260))
GLOBAL_UNIT_ASSIGNED_CONTEXT((#2278,#2280,#2281))
REPRESENTATION_CONTEXT('','3D')
);
#2271=(
GEOMETRIC_REPRESENTATION_CONTEXT(3)
GLOBAL_UNCERTAINTY_ASSIGNED_CONTEXT((#2261))
GLOBAL_UNIT_ASSIGNED_CONTEXT((#2278,#2280,#2281))
REPRESENTATION_CONTEXT('','3D')
);
#2272=(
GEOMETRIC_REPRESENTATION_CONTEXT(3)
GLOBAL_UNCERTAINTY_ASSIGNED_CONTEXT((#2262))
GLOBAL_UNIT_ASSIGNED_CONTEXT((#2278,#2280,#2281))
REPRESENTATION_CONTEXT('','3D')
);
#2273=(
GEOMETRIC_REPRESENTATION_CONTEXT(3)
GLOBAL_UNCERTAINTY_ASSIGNED_CONTEXT((#2263))
GLOBAL_UNIT_ASSIGNED_CONTEXT((#2278,#2280,#2281))
REPRESENTATION_CONTEXT('','3D')
);
#2274=(
GEOMETRIC_REPRESENTATION_CONTEXT(3)
GLOBAL_UNCERTAINTY_ASSIGNED_CONTEXT((#2264))
GLOBAL_UNIT_ASSIGNED_CONTEXT((#2278,#2280,#2281))
REPRESENTATION_CONTEXT('','3D')
);
#2275=(
GEOMETRIC_REPRESENTATION_CONTEXT(3)
GLOBAL_UNCERTAINTY_ASSIGNED_CONTEXT((#2265))
GLOBAL_UNIT_ASSIGNED_CONTEXT((#2278,#2280,#2281))
REPRESENTATION_CONTEXT('','3D')
);
#2276=(
GEOMETRIC_REPRESENTATION_CONTEXT(3)
GLOBAL_UNCERTAINTY_ASSIGNED_CONTEXT((#2266))
GLOBAL_UNIT_ASSIGNED_CONTEXT((#2278,#2280,#2281))
REPRESENTATION_CONTEXT('','3D')
);
#2277=(
GEOMETRIC_REPRESENTATION_CONTEXT(3)
GLOBAL_UNCERTAINTY_ASSIGNED_CONTEXT((#2267))
GLOBAL_UNIT_ASSIGNED_CONTEXT((#2278,#2280,#2281))
REPRESENTATION_CONTEXT('','3D')
);
#2278=(
LENGTH_UNIT()
NAMED_UNIT(*)
SI_UNIT(.CENTI.,.METRE.)
);
#2279=(
LENGTH_UNIT()
NAMED_UNIT(*)
SI_UNIT($,.METRE.)
);
#2280=(
NAMED_UNIT(*)
PLANE_ANGLE_UNIT()
SI_UNIT($,.RADIAN.)
);
#2281=(
NAMED_UNIT(*)
SI_UNIT($,.STERADIAN.)
SOLID_ANGLE_UNIT()
);
#2282=SHAPE_DEFINITION_REPRESENTATION(#2291,#2318);
#2283=SHAPE_DEFINITION_REPRESENTATION(#2292,#2319);
#2284=SHAPE_DEFINITION_REPRESENTATION(#2293,#2320);
#2285=SHAPE_DEFINITION_REPRESENTATION(#2294,#2321);
#2286=SHAPE_DEFINITION_REPRESENTATION(#2295,#2322);
#2287=SHAPE_DEFINITION_REPRESENTATION(#2298,#2323);
#2288=SHAPE_DEFINITION_REPRESENTATION(#2299,#2324);
#2289=SHAPE_DEFINITION_REPRESENTATION(#2300,#2325);
#2290=SHAPE_DEFINITION_REPRESENTATION(#2301,#2326);
#2291=PRODUCT_DEFINITION_SHAPE('',$,#2328);
#2292=PRODUCT_DEFINITION_SHAPE('',$,#2329);
#2293=PRODUCT_DEFINITION_SHAPE('',$,#2330);
#2294=PRODUCT_DEFINITION_SHAPE('',$,#2331);
#2295=PRODUCT_DEFINITION_SHAPE('',$,#2332);
#2296=PRODUCT_DEFINITION_SHAPE($,$,#71);
#2297=PRODUCT_DEFINITION_SHAPE($,$,#72);
#2298=PRODUCT_DEFINITION_SHAPE('',$,#2333);
#2299=PRODUCT_DEFINITION_SHAPE('',$,#2334);
#2300=PRODUCT_DEFINITION_SHAPE('',$,#2335);
#2301=PRODUCT_DEFINITION_SHAPE('',$,#2336);
#2302=PRODUCT_DEFINITION_SHAPE($,$,#73);
#2303=PRODUCT_DEFINITION_SHAPE($,$,#74);
#2304=PRODUCT_DEFINITION_SHAPE($,$,#75);
#2305=PRODUCT_DEFINITION_SHAPE($,$,#76);
#2306=PRODUCT_DEFINITION_SHAPE($,$,#77);
#2307=PRODUCT_DEFINITION_SHAPE($,$,#78);
#2308=PRODUCT_DEFINITION_SHAPE($,$,#79);
#2309=PRODUCT_DEFINITION_SHAPE($,$,#80);
#2310=PRODUCT_DEFINITION_SHAPE($,$,#81);
#2311=PRODUCT_DEFINITION_SHAPE($,$,#82);
#2312=PRODUCT_DEFINITION_SHAPE($,$,#83);
#2313=PRODUCT_DEFINITION_SHAPE($,$,#84);
#2314=PRODUCT_DEFINITION_SHAPE($,$,#85);
#2315=PRODUCT_DEFINITION_SHAPE($,$,#86);
#2316=PRODUCT_DEFINITION_SHAPE($,$,#87);
#2317=PRODUCT_DEFINITION_SHAPE($,$,#88);
#2318=SHAPE_REPRESENTATION('',(#1344,#1484,#1485,#1486,#1487,#1488,#1489,
#1490,#1491,#1492,#1493,#1494,#1495,#1496,#1497,#1498,#1499),#2268);
#2319=SHAPE_REPRESENTATION('',(#1345),#2269);
#2320=SHAPE_REPRESENTATION('',(#1368,#1432,#1433),#2270);
#2321=SHAPE_REPRESENTATION('',(#1369),#2271);
#2322=SHAPE_REPRESENTATION('',(#1410),#2272);
#2323=SHAPE_REPRESENTATION('',(#1434),#2273);
#2324=SHAPE_REPRESENTATION('',(#1443),#2274);
#2325=SHAPE_REPRESENTATION('',(#1452),#2275);
#2326=SHAPE_REPRESENTATION('',(#1478),#2276);
#2327=PRODUCT_DEFINITION_CONTEXT('part definition',#2356,'design');
#2328=PRODUCT_DEFINITION('PAT-112','PAT-112',#2337,#2327);
#2329=PRODUCT_DEFINITION('Mounting base','Mounting base',#2338,#2327);
#2330=PRODUCT_DEFINITION('Pillow Block Bearing - 20 mm Bore',
'Pillow Block Bearing - 20 mm Bore',#2339,#2327);
#2331=PRODUCT_DEFINITION('Housing','Housing',#2340,#2327);
#2332=PRODUCT_DEFINITION('Insert bearing','Insert bearing',#2341,#2327);
#2333=PRODUCT_DEFINITION('Mounting bush','Mounting bush',#2342,#2327);
#2334=PRODUCT_DEFINITION('Flat Washer - M8','Flat Washer - M8',#2343,#2327);
#2335=PRODUCT_DEFINITION('Cap Screw - M8x30','Cap Screw - M8x30',#2344,
#2327);
#2336=PRODUCT_DEFINITION('2026-11-15-15-23-50-266','Shaft',#2345,#2327);
#2337=PRODUCT_DEFINITION_FORMATION('',$,#2358);
#2338=PRODUCT_DEFINITION_FORMATION('',$,#2359);
#2339=PRODUCT_DEFINITION_FORMATION('',$,#2360);
#2340=PRODUCT_DEFINITION_FORMATION('',$,#2361);
#2341=PRODUCT_DEFINITION_FORMATION('',$,#2362);
#2342=PRODUCT_DEFINITION_FORMATION('',$,#2363);
#2343=PRODUCT_DEFINITION_FORMATION('',$,#2364);
#2344=PRODUCT_DEFINITION_FORMATION('',$,#2365);
#2345=PRODUCT_DEFINITION_FORMATION('',$,#2366);
#2346=PRODUCT_RELATED_PRODUCT_CATEGORY('PAT-112','PAT-112',(#2358));
#2347=PRODUCT_RELATED_PRODUCT_CATEGORY('Mounting base','Mounting base',
(#2359));
#2348=PRODUCT_RELATED_PRODUCT_CATEGORY(
'Pillow Block Bearing - 20 mm Bore','Pillow Block Bearing - 20 mm Bore',
(#2360));
#2349=PRODUCT_RELATED_PRODUCT_CATEGORY('Housing','Housing',(#2361));
#2350=PRODUCT_RELATED_PRODUCT_CATEGORY('Insert bearing',
'Insert bearing',(#2362));
#2351=PRODUCT_RELATED_PRODUCT_CATEGORY('Mounting bush','Mounting bush',
(#2363));
#2352=PRODUCT_RELATED_PRODUCT_CATEGORY('Flat Washer - M8',
'Flat Washer - M8',(#2364));
#2353=PRODUCT_RELATED_PRODUCT_CATEGORY('Cap Screw - M8x30',
'Cap Screw - M8x30',(#2365));
#2354=PRODUCT_RELATED_PRODUCT_CATEGORY('Shaft','Shaft',(#2366));
#2355=APPLICATION_PROTOCOL_DEFINITION('international standard',
'automotive_design',2009,#2356);
#2356=APPLICATION_CONTEXT(
'Core Data for Automotive Mechanical Design Process');
#2357=PRODUCT_CONTEXT('part definition',#2356,'mechanical');
#2358=PRODUCT('PAT-112','PAT-112','PAT-112',(#2357));
#2359=PRODUCT('Mounting base','Mounting base','Mounting base',(#2357));
#2360=PRODUCT('Pillow Block Bearing - 20 mm Bore',
'Pillow Block Bearing - 20 mm Bore','Pillow Block Bearing - 20 mm Bore',
(#2357));
#2361=PRODUCT('Housing','Housing','Housing',(#2357));
#2362=PRODUCT('Insert bearing','Insert bearing','Insert bearing',(#2357));
#2363=PRODUCT('Mounting bush','Mounting bush','Mounting bush',(#2357));
#2364=PRODUCT('Flat Washer - M8','Flat Washer - M8','Flat Washer - M8',
(#2357));
#2365=PRODUCT('Cap Screw - M8x30','Cap Screw - M8x30',
'Cap Screw - M8x30',(#2357));
#2366=PRODUCT('2026-11-15-15-23-50-266','Shaft',$,(#2357));
#2367=PRESENTATION_STYLE_ASSIGNMENT((#2372));
#2368=PRESENTATION_STYLE_ASSIGNMENT((#2373));
#2369=PRESENTATION_STYLE_ASSIGNMENT((#2374));
#2370=PRESENTATION_STYLE_ASSIGNMENT((#2375));
#2371=PRESENTATION_STYLE_ASSIGNMENT((#2376));
#2372=SURFACE_STYLE_USAGE(.BOTH.,#2377);
#2373=SURFACE_STYLE_USAGE(.BOTH.,#2378);
#2374=SURFACE_STYLE_USAGE(.BOTH.,#2379);
#2375=SURFACE_STYLE_USAGE(.BOTH.,#2380);
#2376=SURFACE_STYLE_USAGE(.BOTH.,#2381);
#2377=SURFACE_SIDE_STYLE('',(#2382));
#2378=SURFACE_SIDE_STYLE('',(#2383));
#2379=SURFACE_SIDE_STYLE('',(#2384));
#2380=SURFACE_SIDE_STYLE('',(#2385));
#2381=SURFACE_SIDE_STYLE('',(#2386));
#2382=SURFACE_STYLE_FILL_AREA(#2387);
#2383=SURFACE_STYLE_FILL_AREA(#2388);
#2384=SURFACE_STYLE_FILL_AREA(#2389);
#2385=SURFACE_STYLE_FILL_AREA(#2390);
#2386=SURFACE_STYLE_FILL_AREA(#2391);
#2387=FILL_AREA_STYLE('Steel - Satin',(#2392));
#2388=FILL_AREA_STYLE('Opaque(20,51,87)',(#2393));
#2389=FILL_AREA_STYLE('Opaque(122,133,145)',(#2394));
#2390=FILL_AREA_STYLE('Opaque(61,176,222)',(#2395));
#2391=FILL_AREA_STYLE('Opaque(31,36,43)',(#2396));
#2392=FILL_AREA_STYLE_COLOUR('Steel - Satin',#2397);
#2393=FILL_AREA_STYLE_COLOUR('Opaque(20,51,87)',#2398);
#2394=FILL_AREA_STYLE_COLOUR('Opaque(122,133,145)',#2399);
#2395=FILL_AREA_STYLE_COLOUR('Opaque(61,176,222)',#2400);
#2396=FILL_AREA_STYLE_COLOUR('Opaque(31,36,43)',#2401);
#2397=COLOUR_RGB('Steel - Satin',0.627450980392157,0.627450980392157,0.627450980392157);
#2398=COLOUR_RGB('Opaque(20,51,87)',0.0784313725490196,0.2,0.341176470588235);
#2399=COLOUR_RGB('Opaque(122,133,145)',0.47843137254902,0.52156862745098,
0.568627450980392);
#2400=COLOUR_RGB('Opaque(61,176,222)',0.23921568627451,0.690196078431373,
0.870588235294118);
#2401=COLOUR_RGB('Opaque(31,36,43)',0.12156862745098,0.141176470588235,
0.168627450980392);
ENDSEC;
END-ISO-10303-21;
